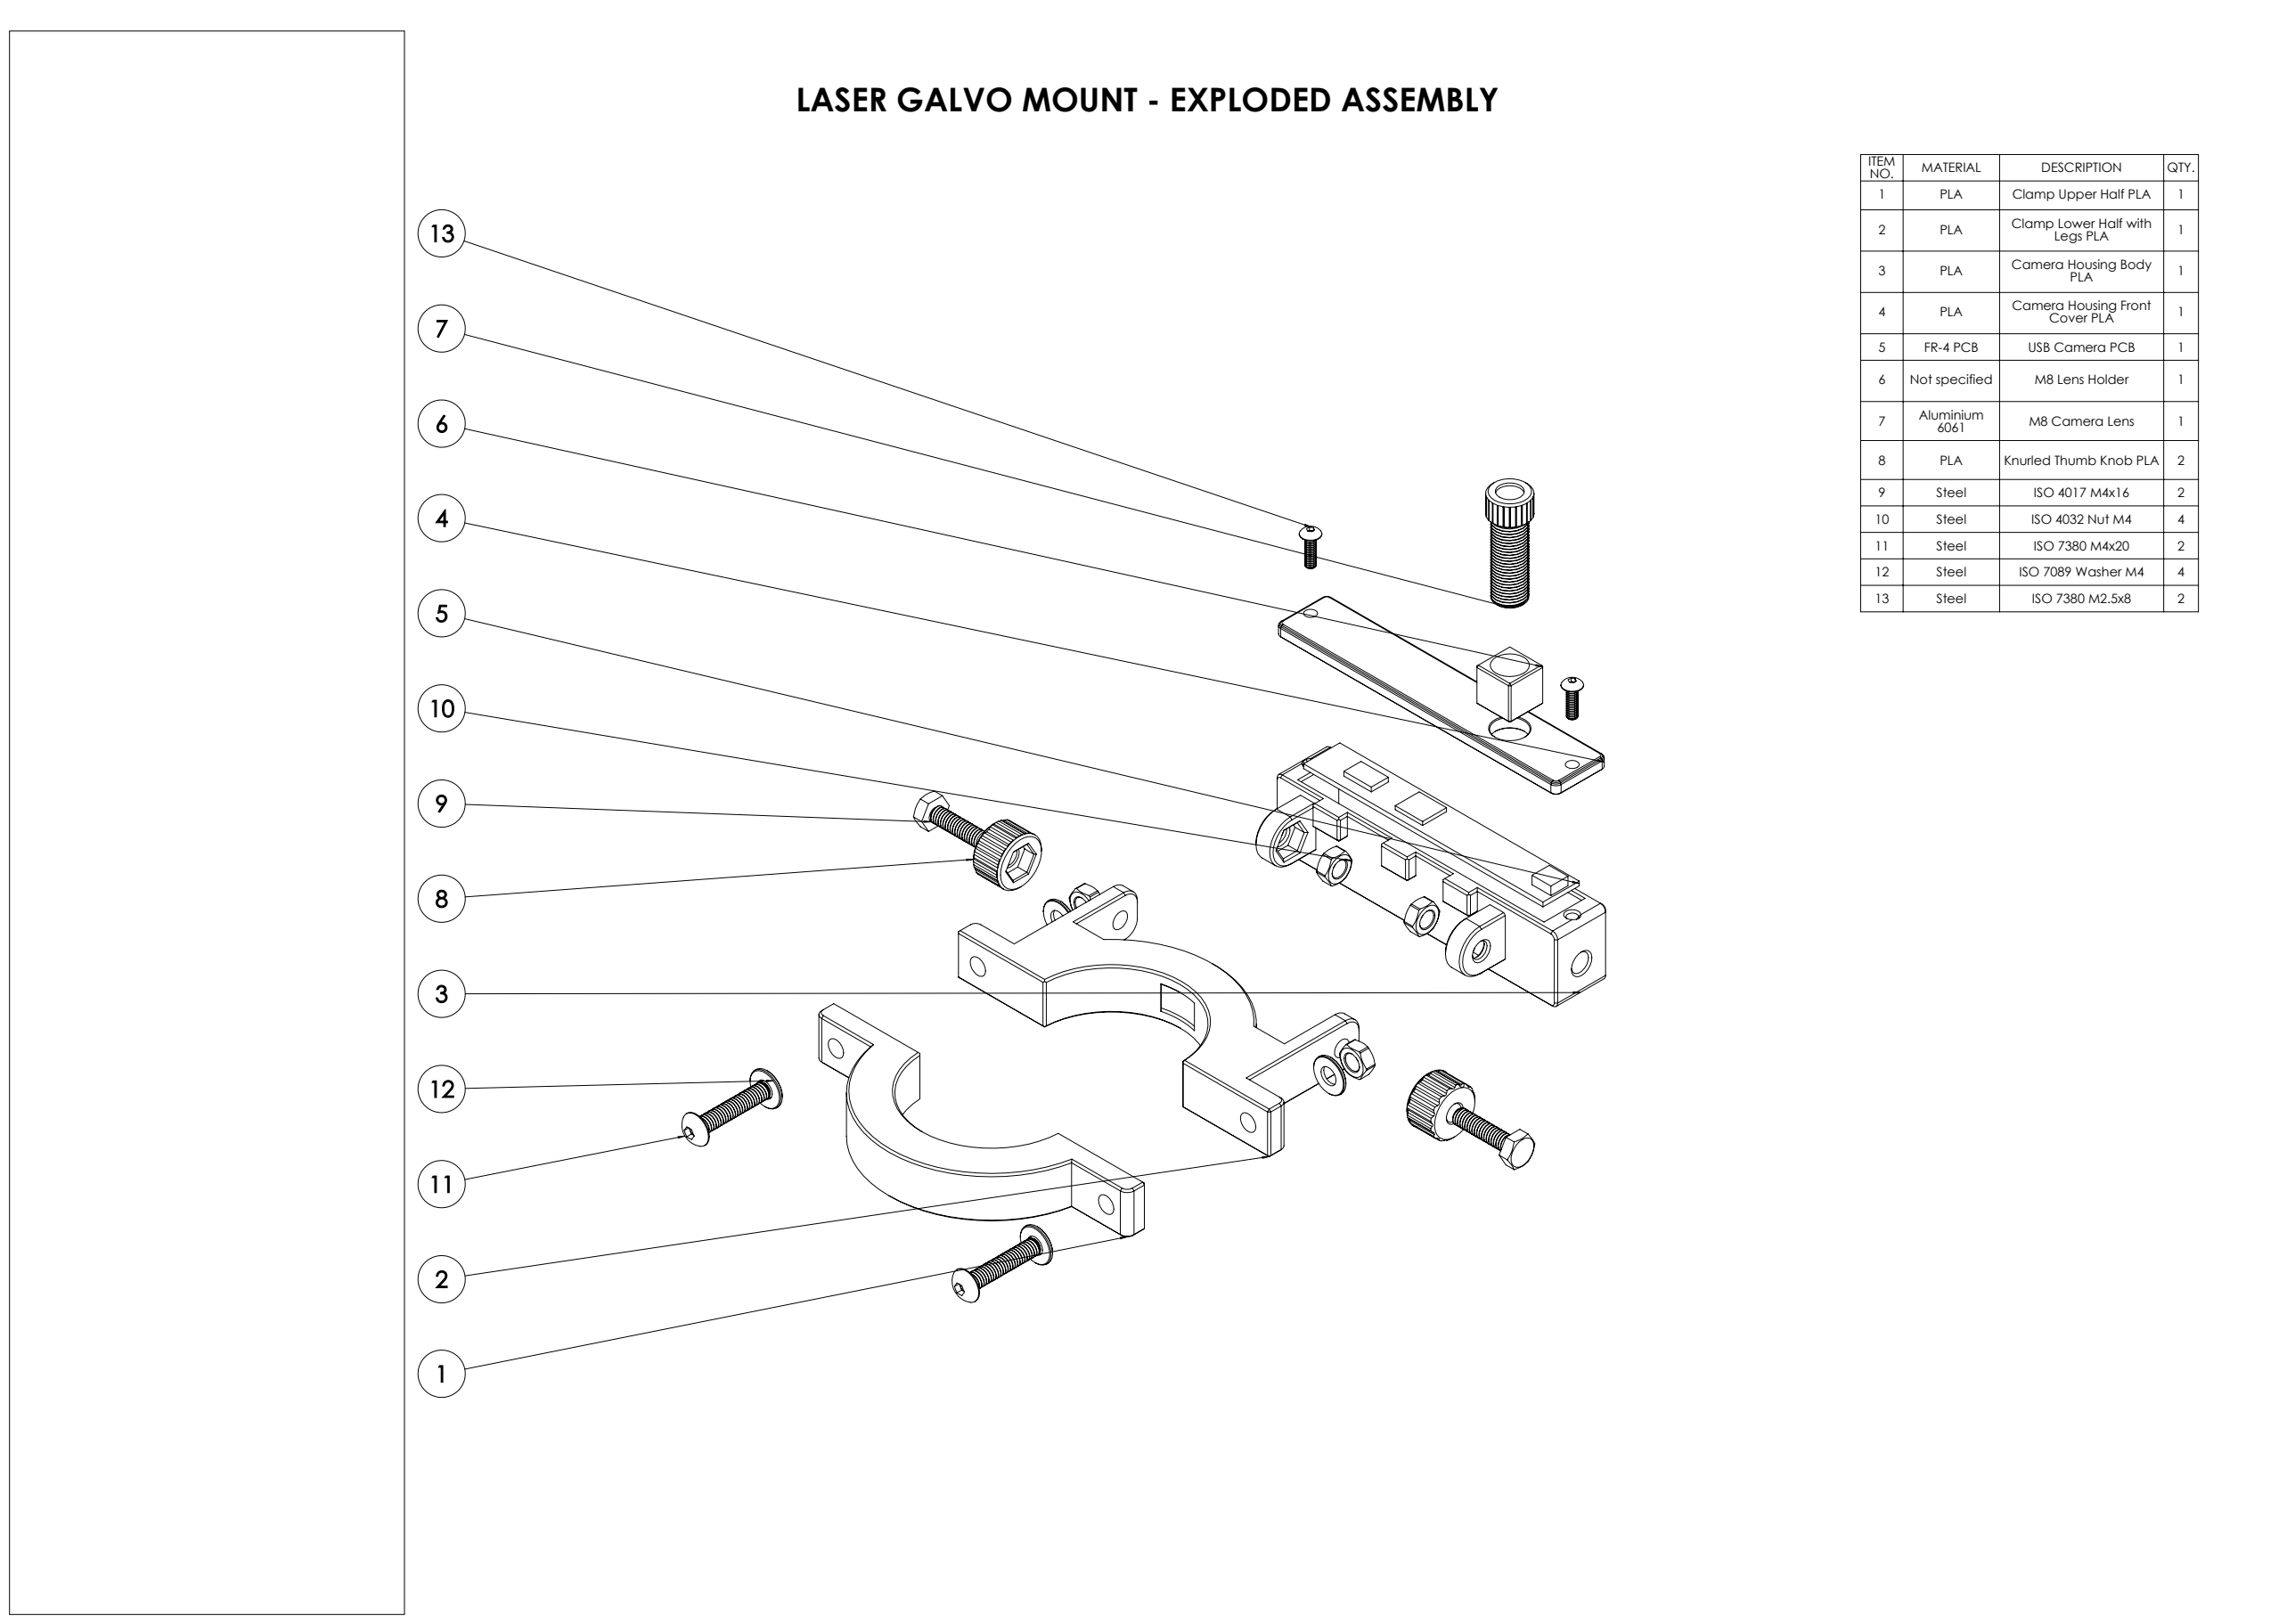
ISO-10303-21;
HEADER;
/* Generated by software containing ST-Developer
 * from STEP Tools, Inc. (www.steptools.com) 
 */

FILE_DESCRIPTION(
/* description */ (''),
/* implementation_level */ '2;1');

FILE_NAME(
/* name */ 'MAS-287',
/* time_stamp */ '2026-10-21T02:01:14-07:00',
/* author */ (''),
/* organization */ (''),
/* preprocessor_version */ 'ST-DEVELOPER v20.2',
/* originating_system */ 'Autodesk Translation Framework v15.15.0.0',
/* authorisation */ '');

FILE_SCHEMA (('AUTOMOTIVE_DESIGN { 1 0 10303 214 3 1 1 }'));
ENDSEC;

DATA;
#10=MECHANICAL_DESIGN_GEOMETRIC_PRESENTATION_REPRESENTATION('',(#614,#615,
#616,#617,#618,#619,#620,#621,#622,#623,#624,#625,#626),#37181);
#11=ITEM_DEFINED_TRANSFORMATION($,$,#14934,#16102);
#12=ITEM_DEFINED_TRANSFORMATION($,$,#14997,#16103);
#13=ITEM_DEFINED_TRANSFORMATION($,$,#15137,#16104);
#14=ITEM_DEFINED_TRANSFORMATION($,$,#15323,#16105);
#15=ITEM_DEFINED_TRANSFORMATION($,$,#15403,#16106);
#16=ITEM_DEFINED_TRANSFORMATION($,$,#15425,#16107);
#17=ITEM_DEFINED_TRANSFORMATION($,$,#15455,#16108);
#18=ITEM_DEFINED_TRANSFORMATION($,$,#15705,#16109);
#19=ITEM_DEFINED_TRANSFORMATION($,$,#15848,#16110);
#20=ITEM_DEFINED_TRANSFORMATION($,$,#16013,#16111);
#21=ITEM_DEFINED_TRANSFORMATION($,$,#15999,#16112);
#22=ITEM_DEFINED_TRANSFORMATION($,$,#15916,#16113);
#23=ITEM_DEFINED_TRANSFORMATION($,$,#15999,#16114);
#24=ITEM_DEFINED_TRANSFORMATION($,$,#16013,#16115);
#25=ITEM_DEFINED_TRANSFORMATION($,$,#15705,#16116);
#26=ITEM_DEFINED_TRANSFORMATION($,$,#15848,#16117);
#27=ITEM_DEFINED_TRANSFORMATION($,$,#16013,#16118);
#28=ITEM_DEFINED_TRANSFORMATION($,$,#15999,#16119);
#29=ITEM_DEFINED_TRANSFORMATION($,$,#15916,#16120);
#30=ITEM_DEFINED_TRANSFORMATION($,$,#15999,#16121);
#31=ITEM_DEFINED_TRANSFORMATION($,$,#16013,#16122);
#32=ITEM_DEFINED_TRANSFORMATION($,$,#16039,#16123);
#33=ITEM_DEFINED_TRANSFORMATION($,$,#16039,#16124);
#34=(
REPRESENTATION_RELATIONSHIP($,$,#37238,#37237)
REPRESENTATION_RELATIONSHIP_WITH_TRANSFORMATION(#11)
SHAPE_REPRESENTATION_RELATIONSHIP()
);
#35=(
REPRESENTATION_RELATIONSHIP($,$,#37239,#37237)
REPRESENTATION_RELATIONSHIP_WITH_TRANSFORMATION(#12)
SHAPE_REPRESENTATION_RELATIONSHIP()
);
#36=(
REPRESENTATION_RELATIONSHIP($,$,#37240,#37237)
REPRESENTATION_RELATIONSHIP_WITH_TRANSFORMATION(#13)
SHAPE_REPRESENTATION_RELATIONSHIP()
);
#37=(
REPRESENTATION_RELATIONSHIP($,$,#37241,#37237)
REPRESENTATION_RELATIONSHIP_WITH_TRANSFORMATION(#14)
SHAPE_REPRESENTATION_RELATIONSHIP()
);
#38=(
REPRESENTATION_RELATIONSHIP($,$,#37242,#37237)
REPRESENTATION_RELATIONSHIP_WITH_TRANSFORMATION(#15)
SHAPE_REPRESENTATION_RELATIONSHIP()
);
#39=(
REPRESENTATION_RELATIONSHIP($,$,#37243,#37237)
REPRESENTATION_RELATIONSHIP_WITH_TRANSFORMATION(#16)
SHAPE_REPRESENTATION_RELATIONSHIP()
);
#40=(
REPRESENTATION_RELATIONSHIP($,$,#37244,#37237)
REPRESENTATION_RELATIONSHIP_WITH_TRANSFORMATION(#17)
SHAPE_REPRESENTATION_RELATIONSHIP()
);
#41=(
REPRESENTATION_RELATIONSHIP($,$,#37245,#37237)
REPRESENTATION_RELATIONSHIP_WITH_TRANSFORMATION(#18)
SHAPE_REPRESENTATION_RELATIONSHIP()
);
#42=(
REPRESENTATION_RELATIONSHIP($,$,#37246,#37237)
REPRESENTATION_RELATIONSHIP_WITH_TRANSFORMATION(#19)
SHAPE_REPRESENTATION_RELATIONSHIP()
);
#43=(
REPRESENTATION_RELATIONSHIP($,$,#37249,#37237)
REPRESENTATION_RELATIONSHIP_WITH_TRANSFORMATION(#20)
SHAPE_REPRESENTATION_RELATIONSHIP()
);
#44=(
REPRESENTATION_RELATIONSHIP($,$,#37248,#37237)
REPRESENTATION_RELATIONSHIP_WITH_TRANSFORMATION(#21)
SHAPE_REPRESENTATION_RELATIONSHIP()
);
#45=(
REPRESENTATION_RELATIONSHIP($,$,#37247,#37237)
REPRESENTATION_RELATIONSHIP_WITH_TRANSFORMATION(#22)
SHAPE_REPRESENTATION_RELATIONSHIP()
);
#46=(
REPRESENTATION_RELATIONSHIP($,$,#37248,#37237)
REPRESENTATION_RELATIONSHIP_WITH_TRANSFORMATION(#23)
SHAPE_REPRESENTATION_RELATIONSHIP()
);
#47=(
REPRESENTATION_RELATIONSHIP($,$,#37249,#37237)
REPRESENTATION_RELATIONSHIP_WITH_TRANSFORMATION(#24)
SHAPE_REPRESENTATION_RELATIONSHIP()
);
#48=(
REPRESENTATION_RELATIONSHIP($,$,#37245,#37237)
REPRESENTATION_RELATIONSHIP_WITH_TRANSFORMATION(#25)
SHAPE_REPRESENTATION_RELATIONSHIP()
);
#49=(
REPRESENTATION_RELATIONSHIP($,$,#37246,#37237)
REPRESENTATION_RELATIONSHIP_WITH_TRANSFORMATION(#26)
SHAPE_REPRESENTATION_RELATIONSHIP()
);
#50=(
REPRESENTATION_RELATIONSHIP($,$,#37249,#37237)
REPRESENTATION_RELATIONSHIP_WITH_TRANSFORMATION(#27)
SHAPE_REPRESENTATION_RELATIONSHIP()
);
#51=(
REPRESENTATION_RELATIONSHIP($,$,#37248,#37237)
REPRESENTATION_RELATIONSHIP_WITH_TRANSFORMATION(#28)
SHAPE_REPRESENTATION_RELATIONSHIP()
);
#52=(
REPRESENTATION_RELATIONSHIP($,$,#37247,#37237)
REPRESENTATION_RELATIONSHIP_WITH_TRANSFORMATION(#29)
SHAPE_REPRESENTATION_RELATIONSHIP()
);
#53=(
REPRESENTATION_RELATIONSHIP($,$,#37248,#37237)
REPRESENTATION_RELATIONSHIP_WITH_TRANSFORMATION(#30)
SHAPE_REPRESENTATION_RELATIONSHIP()
);
#54=(
REPRESENTATION_RELATIONSHIP($,$,#37249,#37237)
REPRESENTATION_RELATIONSHIP_WITH_TRANSFORMATION(#31)
SHAPE_REPRESENTATION_RELATIONSHIP()
);
#55=(
REPRESENTATION_RELATIONSHIP($,$,#37250,#37237)
REPRESENTATION_RELATIONSHIP_WITH_TRANSFORMATION(#32)
SHAPE_REPRESENTATION_RELATIONSHIP()
);
#56=(
REPRESENTATION_RELATIONSHIP($,$,#37250,#37237)
REPRESENTATION_RELATIONSHIP_WITH_TRANSFORMATION(#33)
SHAPE_REPRESENTATION_RELATIONSHIP()
);
#57=CONTEXT_DEPENDENT_SHAPE_REPRESENTATION(#34,#37214);
#58=CONTEXT_DEPENDENT_SHAPE_REPRESENTATION(#35,#37215);
#59=CONTEXT_DEPENDENT_SHAPE_REPRESENTATION(#36,#37216);
#60=CONTEXT_DEPENDENT_SHAPE_REPRESENTATION(#37,#37217);
#61=CONTEXT_DEPENDENT_SHAPE_REPRESENTATION(#38,#37218);
#62=CONTEXT_DEPENDENT_SHAPE_REPRESENTATION(#39,#37219);
#63=CONTEXT_DEPENDENT_SHAPE_REPRESENTATION(#40,#37220);
#64=CONTEXT_DEPENDENT_SHAPE_REPRESENTATION(#41,#37221);
#65=CONTEXT_DEPENDENT_SHAPE_REPRESENTATION(#42,#37222);
#66=CONTEXT_DEPENDENT_SHAPE_REPRESENTATION(#43,#37223);
#67=CONTEXT_DEPENDENT_SHAPE_REPRESENTATION(#44,#37224);
#68=CONTEXT_DEPENDENT_SHAPE_REPRESENTATION(#45,#37225);
#69=CONTEXT_DEPENDENT_SHAPE_REPRESENTATION(#46,#37226);
#70=CONTEXT_DEPENDENT_SHAPE_REPRESENTATION(#47,#37227);
#71=CONTEXT_DEPENDENT_SHAPE_REPRESENTATION(#48,#37228);
#72=CONTEXT_DEPENDENT_SHAPE_REPRESENTATION(#49,#37229);
#73=CONTEXT_DEPENDENT_SHAPE_REPRESENTATION(#50,#37230);
#74=CONTEXT_DEPENDENT_SHAPE_REPRESENTATION(#51,#37231);
#75=CONTEXT_DEPENDENT_SHAPE_REPRESENTATION(#52,#37232);
#76=CONTEXT_DEPENDENT_SHAPE_REPRESENTATION(#53,#37233);
#77=CONTEXT_DEPENDENT_SHAPE_REPRESENTATION(#54,#37234);
#78=CONTEXT_DEPENDENT_SHAPE_REPRESENTATION(#55,#37235);
#79=CONTEXT_DEPENDENT_SHAPE_REPRESENTATION(#56,#37236);
#80=NEXT_ASSEMBLY_USAGE_OCCURRENCE('01_Clamp_Upper_Half_PLA:1',
'01_Clamp_Upper_Half_PLA:1','01_Clamp_Upper_Half_PLA:1',#37252,#37253,
'01_Clamp_Upper_Half_PLA:1');
#81=NEXT_ASSEMBLY_USAGE_OCCURRENCE(
'02_Clamp_Lower_Half_with_Legs_PLA:1',
'02_Clamp_Lower_Half_with_Legs_PLA:1',
'02_Clamp_Lower_Half_with_Legs_PLA:1',#37252,#37254,
'02_Clamp_Lower_Half_with_Legs_PLA:1');
#82=NEXT_ASSEMBLY_USAGE_OCCURRENCE('03_Camera_Housing_Body_PLA:1',
'03_Camera_Housing_Body_PLA:1','03_Camera_Housing_Body_PLA:1',#37252,#37255,
'03_Camera_Housing_Body_PLA:1');
#83=NEXT_ASSEMBLY_USAGE_OCCURRENCE(
'04_Camera_Housing_Front_Cover_PLA:1',
'04_Camera_Housing_Front_Cover_PLA:1',
'04_Camera_Housing_Front_Cover_PLA:1',#37252,#37256,
'04_Camera_Housing_Front_Cover_PLA:1');
#84=NEXT_ASSEMBLY_USAGE_OCCURRENCE('05_USB_Camera_PCB:1',
'05_USB_Camera_PCB:1','05_USB_Camera_PCB:1',#37252,#37257,
'05_USB_Camera_PCB:1');
#85=NEXT_ASSEMBLY_USAGE_OCCURRENCE('06_M8_Lens_Holder:1',
'06_M8_Lens_Holder:1','06_M8_Lens_Holder:1',#37252,#37258,
'06_M8_Lens_Holder:1');
#86=NEXT_ASSEMBLY_USAGE_OCCURRENCE('07_M8_Camera_Lens:2',
'07_M8_Camera_Lens:2','07_M8_Camera_Lens:2',#37252,#37259,
'07_M8_Camera_Lens:2');
#87=NEXT_ASSEMBLY_USAGE_OCCURRENCE('08_Knurled_Thumb_Knob_PLA:2',
'08_Knurled_Thumb_Knob_PLA:2','08_Knurled_Thumb_Knob_PLA:2',#37252,#37260,
'08_Knurled_Thumb_Knob_PLA:2');
#88=NEXT_ASSEMBLY_USAGE_OCCURRENCE('09_ISO_4017_M4x16:2',
'09_ISO_4017_M4x16:2','09_ISO_4017_M4x16:2',#37252,#37261,
'09_ISO_4017_M4x16:2');
#89=NEXT_ASSEMBLY_USAGE_OCCURRENCE('10_ISO_4032_Nut_M4:2',
'10_ISO_4032_Nut_M4:2','10_ISO_4032_Nut_M4:2',#37252,#37264,
'10_ISO_4032_Nut_M4:2');
#90=NEXT_ASSEMBLY_USAGE_OCCURRENCE('12_ISO_7089_Washer_M4:2',
'12_ISO_7089_Washer_M4:2','12_ISO_7089_Washer_M4:2',#37252,#37263,
'12_ISO_7089_Washer_M4:2');
#91=NEXT_ASSEMBLY_USAGE_OCCURRENCE('11_ISO_7380_M4x20:2',
'11_ISO_7380_M4x20:2','11_ISO_7380_M4x20:2',#37252,#37262,
'11_ISO_7380_M4x20:2');
#92=NEXT_ASSEMBLY_USAGE_OCCURRENCE('12_ISO_7089_Washer_M4:3',
'12_ISO_7089_Washer_M4:3','12_ISO_7089_Washer_M4:3',#37252,#37263,
'12_ISO_7089_Washer_M4:3');
#93=NEXT_ASSEMBLY_USAGE_OCCURRENCE('10_ISO_4032_Nut_M4:3',
'10_ISO_4032_Nut_M4:3','10_ISO_4032_Nut_M4:3',#37252,#37264,
'10_ISO_4032_Nut_M4:3');
#94=NEXT_ASSEMBLY_USAGE_OCCURRENCE('08_Knurled_Thumb_Knob_PLA:3',
'08_Knurled_Thumb_Knob_PLA:3','08_Knurled_Thumb_Knob_PLA:3',#37252,#37260,
'08_Knurled_Thumb_Knob_PLA:3');
#95=NEXT_ASSEMBLY_USAGE_OCCURRENCE('09_ISO_4017_M4x16:3',
'09_ISO_4017_M4x16:3','09_ISO_4017_M4x16:3',#37252,#37261,
'09_ISO_4017_M4x16:3');
#96=NEXT_ASSEMBLY_USAGE_OCCURRENCE('10_ISO_4032_Nut_M4:4',
'10_ISO_4032_Nut_M4:4','10_ISO_4032_Nut_M4:4',#37252,#37264,
'10_ISO_4032_Nut_M4:4');
#97=NEXT_ASSEMBLY_USAGE_OCCURRENCE('12_ISO_7089_Washer_M4:4',
'12_ISO_7089_Washer_M4:4','12_ISO_7089_Washer_M4:4',#37252,#37263,
'12_ISO_7089_Washer_M4:4');
#98=NEXT_ASSEMBLY_USAGE_OCCURRENCE('11_ISO_7380_M4x20:3',
'11_ISO_7380_M4x20:3','11_ISO_7380_M4x20:3',#37252,#37262,
'11_ISO_7380_M4x20:3');
#99=NEXT_ASSEMBLY_USAGE_OCCURRENCE('12_ISO_7089_Washer_M4:5',
'12_ISO_7089_Washer_M4:5','12_ISO_7089_Washer_M4:5',#37252,#37263,
'12_ISO_7089_Washer_M4:5');
#100=NEXT_ASSEMBLY_USAGE_OCCURRENCE('10_ISO_4032_Nut_M4:5',
'10_ISO_4032_Nut_M4:5','10_ISO_4032_Nut_M4:5',#37252,#37264,
'10_ISO_4032_Nut_M4:5');
#101=NEXT_ASSEMBLY_USAGE_OCCURRENCE('13_ISO_7380_M2.5x8:2',
'13_ISO_7380_M2.5x8:2','13_ISO_7380_M2.5x8:2',#37252,#37265,
'13_ISO_7380_M2.5x8:2');
#102=NEXT_ASSEMBLY_USAGE_OCCURRENCE('13_ISO_7380_M2.5x8:3',
'13_ISO_7380_M2.5x8:3','13_ISO_7380_M2.5x8:3',#37252,#37265,
'13_ISO_7380_M2.5x8:3');
#103=(
BOUNDED_SURFACE()
B_SPLINE_SURFACE(2,2,((#34249,#34250,#34251,#34252,#34253,#34254,#34255,
#34256,#34257),(#34258,#34259,#34260,#34261,#34262,#34263,#34264,#34265,
#34266),(#34267,#34268,#34269,#34270,#34271,#34272,#34273,#34274,#34275)),
 .UNSPECIFIED.,.F.,.T.,.F.)
B_SPLINE_SURFACE_WITH_KNOTS((3,3),(3,2,2,2,3),(0.516279708895519,1.35421937474488),
(-3.14159265358979,-1.5707963267949,0.,1.5707963267949,3.14159265358979),
 .UNSPECIFIED.)
GEOMETRIC_REPRESENTATION_ITEM()
RATIONAL_B_SPLINE_SURFACE(((1.,0.707106781186548,1.,0.707106781186548,1.,
0.707106781186548,1.,0.707106781186548,1.),(0.91350851712624,0.645948067131631,
0.91350851712624,0.645948067131631,0.91350851712624,0.645948067131631,0.91350851712624,
0.645948067131631,0.91350851712624),(1.,0.707106781186548,1.,0.707106781186548,
1.,0.707106781186548,1.,0.707106781186548,1.)))
REPRESENTATION_ITEM('')
SURFACE()
);
#104=(
BOUNDED_SURFACE()
B_SPLINE_SURFACE(2,2,((#37099,#37100,#37101,#37102,#37103,#37104,#37105,
#37106,#37107),(#37108,#37109,#37110,#37111,#37112,#37113,#37114,#37115,
#37116),(#37117,#37118,#37119,#37120,#37121,#37122,#37123,#37124,#37125)),
 .UNSPECIFIED.,.F.,.T.,.F.)
B_SPLINE_SURFACE_WITH_KNOTS((3,3),(3,2,2,2,3),(0.513408172091738,1.39168804086818),
(-3.14159265358979,-1.5707963267949,0.,1.5707963267949,3.14159265358979),
 .UNSPECIFIED.)
GEOMETRIC_REPRESENTATION_ITEM()
RATIONAL_B_SPLINE_SURFACE(((1.,0.707106781186548,1.,0.707106781186548,1.,
0.707106781186548,1.,0.707106781186548,1.),(0.905117664433204,0.640014838292448,
0.905117664433204,0.640014838292448,0.905117664433204,0.640014838292448,
0.905117664433204,0.640014838292448,0.905117664433204),(1.,0.707106781186548,
1.,0.707106781186548,1.,0.707106781186548,1.,0.707106781186548,1.)))
REPRESENTATION_ITEM('')
SURFACE()
);
#105=B_SPLINE_SURFACE_WITH_KNOTS('',3,3,((#21181,#21182,#21183,#21184,#21185,
#21186),(#21187,#21188,#21189,#21190,#21191,#21192),(#21193,#21194,#21195,
#21196,#21197,#21198),(#21199,#21200,#21201,#21202,#21203,#21204)),
 .UNSPECIFIED.,.F.,.F.,.F.,(4,4),(4,2,4),(0.,1.),(0.268796457448958,0.30404357328347,
0.339290689117984),.UNSPECIFIED.);
#106=B_SPLINE_SURFACE_WITH_KNOTS('',3,3,((#21223,#21224,#21225,#21226),
(#21227,#21228,#21229,#21230),(#21231,#21232,#21233,#21234),(#21235,#21236,
#21237,#21238)),.UNSPECIFIED.,.F.,.F.,.F.,(4,4),(4,4),(0.,1.),(0.278246822734795,
0.803148805386868),.UNSPECIFIED.);
#107=B_SPLINE_SURFACE_WITH_KNOTS('',3,3,((#21243,#21244,#21245,#21246),
(#21247,#21248,#21249,#21250),(#21251,#21252,#21253,#21254),(#21255,#21256,
#21257,#21258)),.UNSPECIFIED.,.F.,.F.,.F.,(4,4),(4,4),(0.,1.),(-0.803148805386867,
-0.278246822734795),.UNSPECIFIED.);
#108=B_SPLINE_SURFACE_WITH_KNOTS('',3,3,((#21267,#21268,#21269,#21270,#21271,
#21272),(#21273,#21274,#21275,#21276,#21277,#21278),(#21279,#21280,#21281,
#21282,#21283,#21284),(#21285,#21286,#21287,#21288,#21289,#21290)),
 .UNSPECIFIED.,.F.,.F.,.F.,(4,4),(4,2,4),(0.,1.),(0.268796457448958,0.304043573283469,
0.33929068911798),.UNSPECIFIED.);
#109=B_SPLINE_SURFACE_WITH_KNOTS('',3,3,((#21310,#21311,#21312,#21313),
(#21314,#21315,#21316,#21317),(#21318,#21319,#21320,#21321),(#21322,#21323,
#21324,#21325)),.UNSPECIFIED.,.F.,.F.,.F.,(4,4),(4,4),(0.,1.),(-2.86334583085503,
-2.33844384820293),.UNSPECIFIED.);
#110=B_SPLINE_SURFACE_WITH_KNOTS('',3,3,((#21330,#21331,#21332,#21333),
(#21334,#21335,#21336,#21337),(#21338,#21339,#21340,#21341),(#21342,#21343,
#21344,#21345)),.UNSPECIFIED.,.F.,.F.,.F.,(4,4),(4,4),(0.,1.),(-3.94474145897665,
-3.41983947632457),.UNSPECIFIED.);
#111=B_SPLINE_SURFACE_WITH_KNOTS('',3,3,((#24257,#24258,#24259,#24260,#24261,
#24262,#24263,#24264,#24265,#24266,#24267,#24268,#24269,#24270,#24271,#24272,
#24273,#24274,#24275,#24276,#24277,#24278,#24279,#24280,#24281,#24282,#24283,
#24284,#24285,#24286,#24287,#24288,#24289,#24290,#24291,#24292,#24293,#24294,
#24295,#24296,#24297,#24298,#24299,#24300,#24301,#24302,#24303,#24304,#24305,
#24306,#24307,#24308,#24309,#24310,#24311,#24312,#24313,#24314,#24315,#24316,
#24317,#24318,#24319,#24320,#24321,#24322,#24323,#24324,#24325,#24326,#24327,
#24328,#24329,#24330,#24331,#24332,#24333,#24334,#24335,#24336,#24337,#24338,
#24339,#24340,#24341,#24342,#24343,#24344,#24345,#24346,#24347,#24348,#24349,
#24350,#24351,#24352,#24353,#24354,#24355,#24356,#24357,#24358,#24359,#24360,
#24361,#24362,#24363,#24364,#24365,#24366,#24367,#24368,#24369,#24370,#24371,
#24372,#24373,#24374,#24375,#24376,#24377,#24378,#24379,#24380,#24381,#24382,
#24383,#24384,#24385,#24386,#24387,#24388,#24389,#24390,#24391,#24392,#24393,
#24394,#24395,#24396,#24397,#24398,#24399,#24400,#24401,#24402,#24403,#24404,
#24405,#24406,#24407,#24408,#24409,#24410,#24411,#24412,#24413,#24414,#24415,
#24416,#24417,#24418,#24419,#24420,#24421,#24422,#24423,#24424,#24425,#24426,
#24427,#24428,#24429,#24430,#24431,#24432,#24433,#24434,#24435),(#24436,
#24437,#24438,#24439,#24440,#24441,#24442,#24443,#24444,#24445,#24446,#24447,
#24448,#24449,#24450,#24451,#24452,#24453,#24454,#24455,#24456,#24457,#24458,
#24459,#24460,#24461,#24462,#24463,#24464,#24465,#24466,#24467,#24468,#24469,
#24470,#24471,#24472,#24473,#24474,#24475,#24476,#24477,#24478,#24479,#24480,
#24481,#24482,#24483,#24484,#24485,#24486,#24487,#24488,#24489,#24490,#24491,
#24492,#24493,#24494,#24495,#24496,#24497,#24498,#24499,#24500,#24501,#24502,
#24503,#24504,#24505,#24506,#24507,#24508,#24509,#24510,#24511,#24512,#24513,
#24514,#24515,#24516,#24517,#24518,#24519,#24520,#24521,#24522,#24523,#24524,
#24525,#24526,#24527,#24528,#24529,#24530,#24531,#24532,#24533,#24534,#24535,
#24536,#24537,#24538,#24539,#24540,#24541,#24542,#24543,#24544,#24545,#24546,
#24547,#24548,#24549,#24550,#24551,#24552,#24553,#24554,#24555,#24556,#24557,
#24558,#24559,#24560,#24561,#24562,#24563,#24564,#24565,#24566,#24567,#24568,
#24569,#24570,#24571,#24572,#24573,#24574,#24575,#24576,#24577,#24578,#24579,
#24580,#24581,#24582,#24583,#24584,#24585,#24586,#24587,#24588,#24589,#24590,
#24591,#24592,#24593,#24594,#24595,#24596,#24597,#24598,#24599,#24600,#24601,
#24602,#24603,#24604,#24605,#24606,#24607,#24608,#24609,#24610,#24611,#24612,
#24613,#24614),(#24615,#24616,#24617,#24618,#24619,#24620,#24621,#24622,
#24623,#24624,#24625,#24626,#24627,#24628,#24629,#24630,#24631,#24632,#24633,
#24634,#24635,#24636,#24637,#24638,#24639,#24640,#24641,#24642,#24643,#24644,
#24645,#24646,#24647,#24648,#24649,#24650,#24651,#24652,#24653,#24654,#24655,
#24656,#24657,#24658,#24659,#24660,#24661,#24662,#24663,#24664,#24665,#24666,
#24667,#24668,#24669,#24670,#24671,#24672,#24673,#24674,#24675,#24676,#24677,
#24678,#24679,#24680,#24681,#24682,#24683,#24684,#24685,#24686,#24687,#24688,
#24689,#24690,#24691,#24692,#24693,#24694,#24695,#24696,#24697,#24698,#24699,
#24700,#24701,#24702,#24703,#24704,#24705,#24706,#24707,#24708,#24709,#24710,
#24711,#24712,#24713,#24714,#24715,#24716,#24717,#24718,#24719,#24720,#24721,
#24722,#24723,#24724,#24725,#24726,#24727,#24728,#24729,#24730,#24731,#24732,
#24733,#24734,#24735,#24736,#24737,#24738,#24739,#24740,#24741,#24742,#24743,
#24744,#24745,#24746,#24747,#24748,#24749,#24750,#24751,#24752,#24753,#24754,
#24755,#24756,#24757,#24758,#24759,#24760,#24761,#24762,#24763,#24764,#24765,
#24766,#24767,#24768,#24769,#24770,#24771,#24772,#24773,#24774,#24775,#24776,
#24777,#24778,#24779,#24780,#24781,#24782,#24783,#24784,#24785,#24786,#24787,
#24788,#24789,#24790,#24791,#24792,#24793),(#24794,#24795,#24796,#24797,
#24798,#24799,#24800,#24801,#24802,#24803,#24804,#24805,#24806,#24807,#24808,
#24809,#24810,#24811,#24812,#24813,#24814,#24815,#24816,#24817,#24818,#24819,
#24820,#24821,#24822,#24823,#24824,#24825,#24826,#24827,#24828,#24829,#24830,
#24831,#24832,#24833,#24834,#24835,#24836,#24837,#24838,#24839,#24840,#24841,
#24842,#24843,#24844,#24845,#24846,#24847,#24848,#24849,#24850,#24851,#24852,
#24853,#24854,#24855,#24856,#24857,#24858,#24859,#24860,#24861,#24862,#24863,
#24864,#24865,#24866,#24867,#24868,#24869,#24870,#24871,#24872,#24873,#24874,
#24875,#24876,#24877,#24878,#24879,#24880,#24881,#24882,#24883,#24884,#24885,
#24886,#24887,#24888,#24889,#24890,#24891,#24892,#24893,#24894,#24895,#24896,
#24897,#24898,#24899,#24900,#24901,#24902,#24903,#24904,#24905,#24906,#24907,
#24908,#24909,#24910,#24911,#24912,#24913,#24914,#24915,#24916,#24917,#24918,
#24919,#24920,#24921,#24922,#24923,#24924,#24925,#24926,#24927,#24928,#24929,
#24930,#24931,#24932,#24933,#24934,#24935,#24936,#24937,#24938,#24939,#24940,
#24941,#24942,#24943,#24944,#24945,#24946,#24947,#24948,#24949,#24950,#24951,
#24952,#24953,#24954,#24955,#24956,#24957,#24958,#24959,#24960,#24961,#24962,
#24963,#24964,#24965,#24966,#24967,#24968,#24969,#24970,#24971,#24972)),
 .UNSPECIFIED.,.F.,.F.,.F.,(4,4),(4,1,1,1,1,1,1,1,1,1,1,1,1,1,1,1,1,1,1,
1,1,1,1,1,1,1,1,1,1,1,1,1,1,1,1,1,1,1,1,1,1,1,1,1,1,1,1,1,1,1,1,1,1,1,1,
1,1,1,1,1,1,1,1,1,1,1,1,1,1,1,1,1,1,1,1,1,1,1,1,1,1,1,1,1,1,1,1,1,1,1,1,
1,1,1,1,1,1,1,1,1,1,1,1,1,1,1,1,1,1,1,1,1,1,1,1,1,1,1,1,1,1,1,1,1,1,1,1,
1,1,1,1,1,1,1,1,1,1,1,1,1,1,1,1,1,1,1,1,1,1,1,1,1,1,1,1,1,1,1,1,1,1,1,1,
1,1,1,1,1,1,1,1,1,1,1,1,1,4),(0.,0.0496809906637673),(8.29514371672438,
9.2897150667619,10.2842864167994,11.2788577668369,12.2734291168745,13.268000466912,
14.2625718169495,15.257143166987,16.2517145170246,17.2462858670621,18.2408572170996,
19.2354285671371,20.2299999171747,21.2245712672122,22.2191426172497,23.2137139672872,
24.2082853173248,25.2028566673623,26.1974280173998,27.1919993674374,28.1865707174749,
29.1811420675124,30.1757134175499,31.1702847675875,32.164856117625,33.1594274676625,
34.1539988177,35.1485701677375,36.1431415177751,37.1377128678126,38.1322842178501,
39.1268555678876,40.1214269179252,41.1159982679627,42.1105696180002,43.1051409680378,
44.0997123180753,45.0942836681128,46.0888550181503,47.0834263681879,48.0779977182254,
49.0725690682629,50.0671404183004,51.061711768338,52.0562831183755,53.050854468413,
54.0454258184505,55.039997168488,56.0345685185256,57.0291398685631,58.0237112186006,
59.0182825686381,60.0128539186757,61.0074252687132,62.0019966187507,62.9965679687882,
63.9911393188258,64.9857106688633,65.9802820189008,66.9748533689383,67.9694247189759,
68.9639960690134,69.9585674190509,70.9531387690884,71.947710119126,72.9422814691635,
73.936852819201,74.9314241692385,75.9259955192761,76.9205668693136,77.9151382193511,
78.9097095693886,79.9042809194262,80.8988522694637,81.8934236195012,82.8879949695387,
83.8825663195763,84.8771376696138,85.8717090196513,86.8662803696888,87.8608517197264,
88.8554230697639,89.8499944198014,90.8445657698389,91.8391371198765,92.833708469914,
93.8282798199515,94.822851169989,95.8174225200266,96.8119938700641,97.8065652201016,
98.8011365701391,99.7957079201767,100.790279270214,101.784850620252,102.779421970289,
103.773993320327,104.768564670364,105.763136020402,106.757707370439,107.752278720477,
108.746850070514,109.741421420552,110.735992770589,111.730564120627,112.725135470664,
113.719706820702,114.71427817074,115.708849520777,116.703420870815,117.697992220852,
118.69256357089,119.687134920927,120.681706270965,121.676277621002,122.67084897104,
123.665420321077,124.659991671115,125.654563021152,126.64913437119,127.643705721227,
128.638277071265,129.632848421302,130.62741977134,131.621991121377,132.616562471415,
133.611133821453,134.60570517149,135.600276521528,136.594847871565,137.589419221603,
138.58399057164,139.578561921678,140.573133271715,141.567704621753,142.56227597179,
143.556847321828,144.551418671865,145.545990021903,146.54056137194,147.535132721978,
148.529704072015,149.524275422053,150.51884677209,151.513418122128,152.507989472165,
153.502560822203,154.497132172241,155.491703522278,156.486274872316,157.480846222353,
158.475417572391,159.469988922428,160.464560272466,161.459131622503,162.453702972541,
163.448274322578,164.442845672616,165.437417022653,166.431988372691,167.426559722728,
168.421131072766,169.415702422803,170.410273772841,171.404845122878,172.399416472916,
173.393987822954,174.388559172991,175.383130523029,176.377701873066,177.372273223104,
178.366844573141,179.361415923179,180.355987273216,181.350558623254,182.345129973291,
183.339701323329),.UNSPECIFIED.);
#112=B_SPLINE_SURFACE_WITH_KNOTS('',3,3,((#25202,#25203,#25204,#25205,#25206,
#25207,#25208,#25209,#25210,#25211,#25212,#25213,#25214,#25215,#25216,#25217,
#25218,#25219,#25220,#25221,#25222,#25223,#25224,#25225,#25226,#25227,#25228,
#25229,#25230,#25231,#25232,#25233,#25234,#25235,#25236,#25237,#25238,#25239,
#25240,#25241,#25242,#25243,#25244,#25245,#25246,#25247,#25248,#25249,#25250,
#25251,#25252,#25253,#25254,#25255,#25256,#25257,#25258,#25259,#25260,#25261,
#25262,#25263,#25264,#25265,#25266,#25267,#25268,#25269,#25270,#25271,#25272,
#25273,#25274,#25275,#25276,#25277,#25278,#25279,#25280,#25281,#25282,#25283,
#25284,#25285,#25286,#25287,#25288,#25289,#25290,#25291,#25292,#25293,#25294,
#25295,#25296,#25297,#25298,#25299,#25300,#25301,#25302,#25303,#25304,#25305,
#25306,#25307,#25308,#25309,#25310,#25311,#25312,#25313,#25314,#25315,#25316,
#25317,#25318,#25319,#25320,#25321,#25322,#25323,#25324,#25325,#25326,#25327,
#25328,#25329,#25330,#25331,#25332,#25333,#25334,#25335,#25336,#25337,#25338,
#25339,#25340,#25341,#25342,#25343,#25344,#25345,#25346,#25347,#25348,#25349,
#25350,#25351,#25352,#25353,#25354,#25355,#25356,#25357,#25358,#25359,#25360,
#25361,#25362,#25363,#25364,#25365,#25366,#25367,#25368,#25369,#25370,#25371,
#25372,#25373,#25374,#25375,#25376,#25377,#25378,#25379,#25380),(#25381,
#25382,#25383,#25384,#25385,#25386,#25387,#25388,#25389,#25390,#25391,#25392,
#25393,#25394,#25395,#25396,#25397,#25398,#25399,#25400,#25401,#25402,#25403,
#25404,#25405,#25406,#25407,#25408,#25409,#25410,#25411,#25412,#25413,#25414,
#25415,#25416,#25417,#25418,#25419,#25420,#25421,#25422,#25423,#25424,#25425,
#25426,#25427,#25428,#25429,#25430,#25431,#25432,#25433,#25434,#25435,#25436,
#25437,#25438,#25439,#25440,#25441,#25442,#25443,#25444,#25445,#25446,#25447,
#25448,#25449,#25450,#25451,#25452,#25453,#25454,#25455,#25456,#25457,#25458,
#25459,#25460,#25461,#25462,#25463,#25464,#25465,#25466,#25467,#25468,#25469,
#25470,#25471,#25472,#25473,#25474,#25475,#25476,#25477,#25478,#25479,#25480,
#25481,#25482,#25483,#25484,#25485,#25486,#25487,#25488,#25489,#25490,#25491,
#25492,#25493,#25494,#25495,#25496,#25497,#25498,#25499,#25500,#25501,#25502,
#25503,#25504,#25505,#25506,#25507,#25508,#25509,#25510,#25511,#25512,#25513,
#25514,#25515,#25516,#25517,#25518,#25519,#25520,#25521,#25522,#25523,#25524,
#25525,#25526,#25527,#25528,#25529,#25530,#25531,#25532,#25533,#25534,#25535,
#25536,#25537,#25538,#25539,#25540,#25541,#25542,#25543,#25544,#25545,#25546,
#25547,#25548,#25549,#25550,#25551,#25552,#25553,#25554,#25555,#25556,#25557,
#25558,#25559),(#25560,#25561,#25562,#25563,#25564,#25565,#25566,#25567,
#25568,#25569,#25570,#25571,#25572,#25573,#25574,#25575,#25576,#25577,#25578,
#25579,#25580,#25581,#25582,#25583,#25584,#25585,#25586,#25587,#25588,#25589,
#25590,#25591,#25592,#25593,#25594,#25595,#25596,#25597,#25598,#25599,#25600,
#25601,#25602,#25603,#25604,#25605,#25606,#25607,#25608,#25609,#25610,#25611,
#25612,#25613,#25614,#25615,#25616,#25617,#25618,#25619,#25620,#25621,#25622,
#25623,#25624,#25625,#25626,#25627,#25628,#25629,#25630,#25631,#25632,#25633,
#25634,#25635,#25636,#25637,#25638,#25639,#25640,#25641,#25642,#25643,#25644,
#25645,#25646,#25647,#25648,#25649,#25650,#25651,#25652,#25653,#25654,#25655,
#25656,#25657,#25658,#25659,#25660,#25661,#25662,#25663,#25664,#25665,#25666,
#25667,#25668,#25669,#25670,#25671,#25672,#25673,#25674,#25675,#25676,#25677,
#25678,#25679,#25680,#25681,#25682,#25683,#25684,#25685,#25686,#25687,#25688,
#25689,#25690,#25691,#25692,#25693,#25694,#25695,#25696,#25697,#25698,#25699,
#25700,#25701,#25702,#25703,#25704,#25705,#25706,#25707,#25708,#25709,#25710,
#25711,#25712,#25713,#25714,#25715,#25716,#25717,#25718,#25719,#25720,#25721,
#25722,#25723,#25724,#25725,#25726,#25727,#25728,#25729,#25730,#25731,#25732,
#25733,#25734,#25735,#25736,#25737,#25738),(#25739,#25740,#25741,#25742,
#25743,#25744,#25745,#25746,#25747,#25748,#25749,#25750,#25751,#25752,#25753,
#25754,#25755,#25756,#25757,#25758,#25759,#25760,#25761,#25762,#25763,#25764,
#25765,#25766,#25767,#25768,#25769,#25770,#25771,#25772,#25773,#25774,#25775,
#25776,#25777,#25778,#25779,#25780,#25781,#25782,#25783,#25784,#25785,#25786,
#25787,#25788,#25789,#25790,#25791,#25792,#25793,#25794,#25795,#25796,#25797,
#25798,#25799,#25800,#25801,#25802,#25803,#25804,#25805,#25806,#25807,#25808,
#25809,#25810,#25811,#25812,#25813,#25814,#25815,#25816,#25817,#25818,#25819,
#25820,#25821,#25822,#25823,#25824,#25825,#25826,#25827,#25828,#25829,#25830,
#25831,#25832,#25833,#25834,#25835,#25836,#25837,#25838,#25839,#25840,#25841,
#25842,#25843,#25844,#25845,#25846,#25847,#25848,#25849,#25850,#25851,#25852,
#25853,#25854,#25855,#25856,#25857,#25858,#25859,#25860,#25861,#25862,#25863,
#25864,#25865,#25866,#25867,#25868,#25869,#25870,#25871,#25872,#25873,#25874,
#25875,#25876,#25877,#25878,#25879,#25880,#25881,#25882,#25883,#25884,#25885,
#25886,#25887,#25888,#25889,#25890,#25891,#25892,#25893,#25894,#25895,#25896,
#25897,#25898,#25899,#25900,#25901,#25902,#25903,#25904,#25905,#25906,#25907,
#25908,#25909,#25910,#25911,#25912,#25913,#25914,#25915,#25916,#25917)),
 .UNSPECIFIED.,.F.,.F.,.F.,(4,4),(4,1,1,1,1,1,1,1,1,1,1,1,1,1,1,1,1,1,1,
1,1,1,1,1,1,1,1,1,1,1,1,1,1,1,1,1,1,1,1,1,1,1,1,1,1,1,1,1,1,1,1,1,1,1,1,
1,1,1,1,1,1,1,1,1,1,1,1,1,1,1,1,1,1,1,1,1,1,1,1,1,1,1,1,1,1,1,1,1,1,1,1,
1,1,1,1,1,1,1,1,1,1,1,1,1,1,1,1,1,1,1,1,1,1,1,1,1,1,1,1,1,1,1,1,1,1,1,1,
1,1,1,1,1,1,1,1,1,1,1,1,1,1,1,1,1,1,1,1,1,1,1,1,1,1,1,1,1,1,1,1,1,1,1,1,
1,1,1,1,1,1,1,1,1,1,1,1,1,4),(0.,0.0496809906637673),(11.6149723878396,
12.6095437378771,13.6041150879146,14.5986864379522,15.5932577879897,16.5878291380272,
17.5824004880647,18.5769718381023,19.5715431881398,20.5661145381773,21.5606858882148,
22.5552572382524,23.5498285882899,24.5443999383274,25.5389712883649,26.5335426384025,
27.52811398844,28.5226853384775,29.517256688515,30.5118280385526,31.5063993885901,
32.5009707386276,33.4955420886651,34.4901134387027,35.4846847887402,36.4792561387777,
37.4738274888152,38.4683988388528,39.4629701888903,40.4575415389278,41.4521128889653,
42.4466842390029,43.4412555890404,44.4358269390779,45.4303982891154,46.424969639153,
47.4195409891905,48.414112339228,49.4086836892655,50.4032550393031,51.3978263893406,
52.3923977393781,53.3869690894156,54.3815404394532,55.3761117894907,56.3706831395282,
57.3652544895657,58.3598258396033,59.3543971896408,60.3489685396783,61.3435398897158,
62.3381112397534,63.3326825897909,64.3272539398284,65.3218252898659,66.3163966399035,
67.310967989941,68.3055393399785,69.300110690016,70.2946820400536,71.2892533900911,
72.2838247401286,73.2783960901661,74.2729674402037,75.2675387902412,76.2621101402787,
77.2566814903162,78.2512528403538,79.2458241903913,80.2403955404288,81.2349668904663,
82.2295382405039,83.2241095905414,84.2186809405789,85.2132522906164,86.207823640654,
87.2023949906915,88.196966340729,89.1915376907665,90.1861090408041,91.1806803908416,
92.1752517408791,93.1698230909166,94.1643944409542,95.1589657909917,96.1535371410292,
97.1481084910667,98.1426798411043,99.1372511911418,100.131822541179,101.126393891217,
102.120965241254,103.115536591292,104.110107941329,105.104679291367,106.099250641404,
107.093821991442,108.08839334148,109.082964691517,110.077536041555,111.072107391592,
112.06667874163,113.061250091667,114.055821441705,115.050392791742,116.04496414178,
117.039535491817,118.034106841855,119.028678191892,120.02324954193,121.017820891967,
122.012392242005,123.006963592042,124.00153494208,124.996106292117,125.990677642155,
126.985248992192,127.97982034223,128.974391692268,129.968963042305,130.963534392343,
131.95810574238,132.952677092418,133.947248442455,134.941819792493,135.93639114253,
136.930962492568,137.925533842605,138.920105192643,139.91467654268,140.909247892718,
141.903819242755,142.898390592793,143.89296194283,144.887533292868,145.882104642905,
146.876675992943,147.87124734298,148.865818693018,149.860390043056,150.854961393093,
151.849532743131,152.844104093168,153.838675443206,154.833246793243,155.827818143281,
156.822389493318,157.816960843356,158.811532193393,159.806103543431,160.800674893468,
161.795246243506,162.789817593543,163.784388943581,164.778960293618,165.773531643656,
166.768102993693,167.762674343731,168.757245693769,169.751817043806,170.746388393844,
171.740959743881,172.735531093919,173.730102443956,174.724673793994,175.719245144031,
176.713816494069,177.708387844106,178.702959194144,179.697530544181,180.692101894219,
181.686673244256,182.681244594294,183.675815944331,184.670387294369,185.664958644406,
186.659529994444),.UNSPECIFIED.);
#113=B_SPLINE_SURFACE_WITH_KNOTS('',3,3,((#26771,#26772,#26773,#26774,#26775,
#26776,#26777,#26778,#26779),(#26780,#26781,#26782,#26783,#26784,#26785,
#26786,#26787,#26788),(#26789,#26790,#26791,#26792,#26793,#26794,#26795,
#26796,#26797),(#26798,#26799,#26800,#26801,#26802,#26803,#26804,#26805,
#26806)),.UNSPECIFIED.,.F.,.F.,.F.,(4,4),(4,1,1,1,1,1,4),(0.,1.),(0.0342009647377285,
0.0587640238978664,0.0833270830580044,0.107890142218142,0.13245320137828,
0.181579319698556,0.206142378858694),.UNSPECIFIED.);
#114=B_SPLINE_SURFACE_WITH_KNOTS('',3,3,((#28629,#28630,#28631,#28632,#28633,
#28634,#28635,#28636,#28637,#28638,#28639,#28640,#28641,#28642,#28643,#28644,
#28645,#28646,#28647,#28648,#28649,#28650,#28651,#28652,#28653,#28654,#28655,
#28656,#28657,#28658,#28659,#28660,#28661,#28662,#28663,#28664,#28665,#28666,
#28667,#28668,#28669,#28670,#28671,#28672,#28673,#28674,#28675,#28676,#28677,
#28678,#28679,#28680,#28681,#28682,#28683,#28684,#28685,#28686,#28687,#28688,
#28689,#28690,#28691,#28692,#28693,#28694,#28695,#28696,#28697,#28698,#28699,
#28700,#28701,#28702,#28703,#28704,#28705,#28706,#28707,#28708,#28709,#28710,
#28711,#28712,#28713,#28714,#28715,#28716,#28717,#28718,#28719,#28720,#28721,
#28722,#28723,#28724,#28725,#28726,#28727,#28728,#28729,#28730,#28731,#28732,
#28733,#28734,#28735,#28736,#28737,#28738,#28739,#28740,#28741,#28742,#28743,
#28744,#28745,#28746,#28747,#28748,#28749,#28750,#28751,#28752,#28753,#28754,
#28755,#28756,#28757,#28758,#28759,#28760,#28761,#28762,#28763,#28764,#28765,
#28766,#28767,#28768,#28769,#28770,#28771,#28772,#28773,#28774),(#28775,
#28776,#28777,#28778,#28779,#28780,#28781,#28782,#28783,#28784,#28785,#28786,
#28787,#28788,#28789,#28790,#28791,#28792,#28793,#28794,#28795,#28796,#28797,
#28798,#28799,#28800,#28801,#28802,#28803,#28804,#28805,#28806,#28807,#28808,
#28809,#28810,#28811,#28812,#28813,#28814,#28815,#28816,#28817,#28818,#28819,
#28820,#28821,#28822,#28823,#28824,#28825,#28826,#28827,#28828,#28829,#28830,
#28831,#28832,#28833,#28834,#28835,#28836,#28837,#28838,#28839,#28840,#28841,
#28842,#28843,#28844,#28845,#28846,#28847,#28848,#28849,#28850,#28851,#28852,
#28853,#28854,#28855,#28856,#28857,#28858,#28859,#28860,#28861,#28862,#28863,
#28864,#28865,#28866,#28867,#28868,#28869,#28870,#28871,#28872,#28873,#28874,
#28875,#28876,#28877,#28878,#28879,#28880,#28881,#28882,#28883,#28884,#28885,
#28886,#28887,#28888,#28889,#28890,#28891,#28892,#28893,#28894,#28895,#28896,
#28897,#28898,#28899,#28900,#28901,#28902,#28903,#28904,#28905,#28906,#28907,
#28908,#28909,#28910,#28911,#28912,#28913,#28914,#28915,#28916,#28917,#28918,
#28919,#28920),(#28921,#28922,#28923,#28924,#28925,#28926,#28927,#28928,
#28929,#28930,#28931,#28932,#28933,#28934,#28935,#28936,#28937,#28938,#28939,
#28940,#28941,#28942,#28943,#28944,#28945,#28946,#28947,#28948,#28949,#28950,
#28951,#28952,#28953,#28954,#28955,#28956,#28957,#28958,#28959,#28960,#28961,
#28962,#28963,#28964,#28965,#28966,#28967,#28968,#28969,#28970,#28971,#28972,
#28973,#28974,#28975,#28976,#28977,#28978,#28979,#28980,#28981,#28982,#28983,
#28984,#28985,#28986,#28987,#28988,#28989,#28990,#28991,#28992,#28993,#28994,
#28995,#28996,#28997,#28998,#28999,#29000,#29001,#29002,#29003,#29004,#29005,
#29006,#29007,#29008,#29009,#29010,#29011,#29012,#29013,#29014,#29015,#29016,
#29017,#29018,#29019,#29020,#29021,#29022,#29023,#29024,#29025,#29026,#29027,
#29028,#29029,#29030,#29031,#29032,#29033,#29034,#29035,#29036,#29037,#29038,
#29039,#29040,#29041,#29042,#29043,#29044,#29045,#29046,#29047,#29048,#29049,
#29050,#29051,#29052,#29053,#29054,#29055,#29056,#29057,#29058,#29059,#29060,
#29061,#29062,#29063,#29064,#29065,#29066),(#29067,#29068,#29069,#29070,
#29071,#29072,#29073,#29074,#29075,#29076,#29077,#29078,#29079,#29080,#29081,
#29082,#29083,#29084,#29085,#29086,#29087,#29088,#29089,#29090,#29091,#29092,
#29093,#29094,#29095,#29096,#29097,#29098,#29099,#29100,#29101,#29102,#29103,
#29104,#29105,#29106,#29107,#29108,#29109,#29110,#29111,#29112,#29113,#29114,
#29115,#29116,#29117,#29118,#29119,#29120,#29121,#29122,#29123,#29124,#29125,
#29126,#29127,#29128,#29129,#29130,#29131,#29132,#29133,#29134,#29135,#29136,
#29137,#29138,#29139,#29140,#29141,#29142,#29143,#29144,#29145,#29146,#29147,
#29148,#29149,#29150,#29151,#29152,#29153,#29154,#29155,#29156,#29157,#29158,
#29159,#29160,#29161,#29162,#29163,#29164,#29165,#29166,#29167,#29168,#29169,
#29170,#29171,#29172,#29173,#29174,#29175,#29176,#29177,#29178,#29179,#29180,
#29181,#29182,#29183,#29184,#29185,#29186,#29187,#29188,#29189,#29190,#29191,
#29192,#29193,#29194,#29195,#29196,#29197,#29198,#29199,#29200,#29201,#29202,
#29203,#29204,#29205,#29206,#29207,#29208,#29209,#29210,#29211,#29212)),
 .UNSPECIFIED.,.F.,.F.,.F.,(4,4),(4,1,1,1,1,1,1,1,1,1,1,1,1,1,1,1,1,1,1,
1,1,1,1,1,1,1,1,1,1,1,1,1,1,1,1,1,1,1,1,1,1,1,1,1,1,1,1,1,1,1,1,1,1,1,1,
1,1,1,1,1,1,1,1,1,1,1,1,1,1,1,1,1,1,1,1,1,1,1,1,1,1,1,1,1,1,1,1,1,1,1,1,
1,1,1,1,1,1,1,1,1,1,1,1,1,1,1,1,1,1,1,1,1,1,1,1,1,1,1,1,1,1,1,1,1,1,1,1,
1,1,1,1,1,1,1,1,1,1,1,1,1,1,1,1,4),(0.,0.0460148164544131),(8.31058692273977,
9.30711355020657,10.3036401776734,11.3001668051402,12.296693432607,13.2932200600738,
14.2897466875406,15.2862733150074,16.2827999424742,17.279326569941,18.2758531974078,
19.2723798248745,20.2689064523413,21.2654330798081,22.2619597072749,23.2584863347417,
24.2550129622085,25.2515395896753,26.2480662171421,27.2445928446089,28.2411194720757,
29.2376460995425,30.2341727270093,31.2306993544761,32.2272259819429,33.2237526094097,
34.2202792368765,35.2168058643433,36.2133324918101,37.2098591192769,38.2063857467437,
39.2029123742105,40.1994390016773,41.1959656291441,42.1924922566109,43.1890188840777,
44.1855455115445,45.1820721390113,46.1785987664781,47.1751253939449,48.1716520214117,
49.1681786488785,50.1647052763453,51.1612319038121,52.1577585312789,53.1542851587457,
54.1508117862125,55.1473384136793,56.1438650411461,57.1403916686129,58.1369182960797,
59.1334449235465,60.1299715510133,61.1264981784801,62.1230248059469,63.1195514334137,
64.1160780608805,65.1126046883473,66.1091313158141,67.1056579432809,68.1021845707477,
69.0987111982145,70.0952378256813,71.0917644531481,72.0882910806149,73.0848177080817,
74.0813443355485,75.0778709630153,76.0743975904821,77.0709242179488,78.0674508454156,
79.0639774728824,80.0605041003492,81.057030727816,82.0535573552828,83.0500839827496,
84.0466106102164,85.0431372376832,86.03966386515,87.0361904926168,88.0327171200836,
89.0292437475504,90.0257703750172,91.022297002484,92.0188236299508,93.0153502574176,
94.0118768848844,95.0084035123512,96.004930139818,97.0014567672848,97.9979833947516,
98.9945100222184,99.9910366496852,100.987563277152,101.984089904619,102.980616532086,
103.977143159552,104.973669787019,105.970196414486,106.966723041953,107.96324966942,
108.959776296886,109.956302924353,110.95282955182,111.949356179287,112.945882806754,
113.94240943422,114.938936061687,115.935462689154,116.931989316621,117.928515944088,
118.925042571554,119.921569199021,120.918095826488,121.914622453955,122.911149081422,
123.907675708888,124.904202336355,125.900728963822,126.897255591289,127.893782218756,
128.890308846222,129.886835473689,130.883362101156,131.879888728623,132.87641535609,
133.872941983556,134.869468611023,135.86599523849,136.862521865957,137.859048493424,
138.85557512089,139.852101748357,140.848628375824,141.845155003291,142.841681630758,
143.838208258224,144.834734885691,145.831261513158,146.827788140625,147.824314768092,
148.820841395558,149.817368023025,150.813894650492),.UNSPECIFIED.);
#115=B_SPLINE_SURFACE_WITH_KNOTS('',3,3,((#29504,#29505,#29506,#29507,#29508,
#29509,#29510,#29511,#29512,#29513,#29514,#29515,#29516,#29517,#29518,#29519,
#29520,#29521,#29522,#29523,#29524,#29525,#29526,#29527,#29528,#29529,#29530,
#29531,#29532,#29533,#29534,#29535,#29536,#29537,#29538,#29539,#29540,#29541,
#29542,#29543,#29544,#29545,#29546,#29547,#29548,#29549,#29550,#29551,#29552,
#29553,#29554,#29555,#29556,#29557,#29558,#29559,#29560,#29561,#29562,#29563,
#29564,#29565,#29566,#29567,#29568,#29569,#29570,#29571,#29572,#29573,#29574,
#29575,#29576,#29577,#29578,#29579,#29580,#29581,#29582,#29583,#29584,#29585,
#29586,#29587,#29588,#29589,#29590,#29591,#29592,#29593,#29594,#29595,#29596,
#29597,#29598,#29599,#29600,#29601,#29602,#29603,#29604,#29605,#29606,#29607,
#29608,#29609,#29610,#29611,#29612,#29613,#29614,#29615,#29616,#29617,#29618,
#29619,#29620,#29621,#29622,#29623,#29624,#29625,#29626,#29627,#29628,#29629,
#29630,#29631,#29632,#29633,#29634,#29635,#29636,#29637,#29638,#29639,#29640,
#29641,#29642,#29643,#29644,#29645,#29646,#29647,#29648,#29649),(#29650,
#29651,#29652,#29653,#29654,#29655,#29656,#29657,#29658,#29659,#29660,#29661,
#29662,#29663,#29664,#29665,#29666,#29667,#29668,#29669,#29670,#29671,#29672,
#29673,#29674,#29675,#29676,#29677,#29678,#29679,#29680,#29681,#29682,#29683,
#29684,#29685,#29686,#29687,#29688,#29689,#29690,#29691,#29692,#29693,#29694,
#29695,#29696,#29697,#29698,#29699,#29700,#29701,#29702,#29703,#29704,#29705,
#29706,#29707,#29708,#29709,#29710,#29711,#29712,#29713,#29714,#29715,#29716,
#29717,#29718,#29719,#29720,#29721,#29722,#29723,#29724,#29725,#29726,#29727,
#29728,#29729,#29730,#29731,#29732,#29733,#29734,#29735,#29736,#29737,#29738,
#29739,#29740,#29741,#29742,#29743,#29744,#29745,#29746,#29747,#29748,#29749,
#29750,#29751,#29752,#29753,#29754,#29755,#29756,#29757,#29758,#29759,#29760,
#29761,#29762,#29763,#29764,#29765,#29766,#29767,#29768,#29769,#29770,#29771,
#29772,#29773,#29774,#29775,#29776,#29777,#29778,#29779,#29780,#29781,#29782,
#29783,#29784,#29785,#29786,#29787,#29788,#29789,#29790,#29791,#29792,#29793,
#29794,#29795),(#29796,#29797,#29798,#29799,#29800,#29801,#29802,#29803,
#29804,#29805,#29806,#29807,#29808,#29809,#29810,#29811,#29812,#29813,#29814,
#29815,#29816,#29817,#29818,#29819,#29820,#29821,#29822,#29823,#29824,#29825,
#29826,#29827,#29828,#29829,#29830,#29831,#29832,#29833,#29834,#29835,#29836,
#29837,#29838,#29839,#29840,#29841,#29842,#29843,#29844,#29845,#29846,#29847,
#29848,#29849,#29850,#29851,#29852,#29853,#29854,#29855,#29856,#29857,#29858,
#29859,#29860,#29861,#29862,#29863,#29864,#29865,#29866,#29867,#29868,#29869,
#29870,#29871,#29872,#29873,#29874,#29875,#29876,#29877,#29878,#29879,#29880,
#29881,#29882,#29883,#29884,#29885,#29886,#29887,#29888,#29889,#29890,#29891,
#29892,#29893,#29894,#29895,#29896,#29897,#29898,#29899,#29900,#29901,#29902,
#29903,#29904,#29905,#29906,#29907,#29908,#29909,#29910,#29911,#29912,#29913,
#29914,#29915,#29916,#29917,#29918,#29919,#29920,#29921,#29922,#29923,#29924,
#29925,#29926,#29927,#29928,#29929,#29930,#29931,#29932,#29933,#29934,#29935,
#29936,#29937,#29938,#29939,#29940,#29941),(#29942,#29943,#29944,#29945,
#29946,#29947,#29948,#29949,#29950,#29951,#29952,#29953,#29954,#29955,#29956,
#29957,#29958,#29959,#29960,#29961,#29962,#29963,#29964,#29965,#29966,#29967,
#29968,#29969,#29970,#29971,#29972,#29973,#29974,#29975,#29976,#29977,#29978,
#29979,#29980,#29981,#29982,#29983,#29984,#29985,#29986,#29987,#29988,#29989,
#29990,#29991,#29992,#29993,#29994,#29995,#29996,#29997,#29998,#29999,#30000,
#30001,#30002,#30003,#30004,#30005,#30006,#30007,#30008,#30009,#30010,#30011,
#30012,#30013,#30014,#30015,#30016,#30017,#30018,#30019,#30020,#30021,#30022,
#30023,#30024,#30025,#30026,#30027,#30028,#30029,#30030,#30031,#30032,#30033,
#30034,#30035,#30036,#30037,#30038,#30039,#30040,#30041,#30042,#30043,#30044,
#30045,#30046,#30047,#30048,#30049,#30050,#30051,#30052,#30053,#30054,#30055,
#30056,#30057,#30058,#30059,#30060,#30061,#30062,#30063,#30064,#30065,#30066,
#30067,#30068,#30069,#30070,#30071,#30072,#30073,#30074,#30075,#30076,#30077,
#30078,#30079,#30080,#30081,#30082,#30083,#30084,#30085,#30086,#30087)),
 .UNSPECIFIED.,.F.,.F.,.F.,(4,4),(4,1,1,1,1,1,1,1,1,1,1,1,1,1,1,1,1,1,1,
1,1,1,1,1,1,1,1,1,1,1,1,1,1,1,1,1,1,1,1,1,1,1,1,1,1,1,1,1,1,1,1,1,1,1,1,
1,1,1,1,1,1,1,1,1,1,1,1,1,1,1,1,1,1,1,1,1,1,1,1,1,1,1,1,1,1,1,1,1,1,1,1,
1,1,1,1,1,1,1,1,1,1,1,1,1,1,1,1,1,1,1,1,1,1,1,1,1,1,1,1,1,1,1,1,1,1,1,1,
1,1,1,1,1,1,1,1,1,1,1,1,1,1,1,1,4),(0.,0.0460148164544131),(11.6154215191106,
12.6119481465774,13.6084747740442,14.605001401511,15.6015280289778,16.5980546564446,
17.5945812839114,18.5911079113782,19.587634538845,20.5841611663118,21.5806877937786,
22.5772144212454,23.5737410487122,24.570267676179,25.5667943036458,26.5633209311126,
27.5598475585794,28.5563741860462,29.552900813513,30.5494274409798,31.5459540684466,
32.5424806959134,33.5390073233802,34.535533950847,35.5320605783138,36.5285872057806,
37.5251138332474,38.5216404607142,39.518167088181,40.5146937156478,41.5112203431146,
42.5077469705814,43.5042735980482,44.500800225515,45.4973268529818,46.4938534804486,
47.4903801079154,48.4869067353822,49.483433362849,50.4799599903158,51.4764866177826,
52.4730132452493,53.4695398727161,54.4660665001829,55.4625931276497,56.4591197551165,
57.4556463825833,58.4521730100501,59.4486996375169,60.4452262649837,61.4417528924505,
62.4382795199173,63.4348061473841,64.4313327748509,65.4278594023177,66.4243860297845,
67.4209126572513,68.4174392847181,69.4139659121849,70.4104925396517,71.4070191671185,
72.4035457945853,73.4000724220521,74.3965990495189,75.3931256769857,76.3896523044525,
77.3861789319193,78.3827055593861,79.3792321868529,80.3757588143197,81.3722854417865,
82.3688120692533,83.3653386967201,84.3618653241869,85.3583919516537,86.3549185791205,
87.3514452065873,88.3479718340541,89.3444984615209,90.3410250889877,91.3375517164545,
92.3340783439213,93.3306049713881,94.3271315988549,95.3236582263217,96.3201848537885,
97.3167114812553,98.313238108722,99.3097647361889,100.306291363656,101.302817991122,
102.299344618589,103.295871246056,104.292397873523,105.28892450099,106.285451128456,
107.281977755923,108.27850438339,109.275031010857,110.271557638324,111.26808426579,
112.264610893257,113.261137520724,114.257664148191,115.254190775658,116.250717403124,
117.247244030591,118.243770658058,119.240297285525,120.236823912992,121.233350540458,
122.229877167925,123.226403795392,124.222930422859,125.219457050326,126.215983677792,
127.212510305259,128.209036932726,129.205563560193,130.20209018766,131.198616815126,
132.195143442593,133.19167007006,134.188196697527,135.184723324994,136.18124995246,
137.177776579927,138.174303207394,139.170829834861,140.167356462328,141.163883089794,
142.160409717261,143.156936344728,144.153462972195,145.149989599662,146.146516227128,
147.143042854595,148.139569482062,149.136096109529,150.132622736996,151.129149364462,
152.125675991929,153.122202619396,154.118729246863),.UNSPECIFIED.);
#116=B_SPLINE_SURFACE_WITH_KNOTS('',3,3,((#32297,#32298,#32299,#32300,#32301,
#32302,#32303,#32304,#32305,#32306,#32307,#32308,#32309,#32310,#32311,#32312,
#32313,#32314,#32315,#32316,#32317,#32318,#32319,#32320,#32321,#32322,#32323,
#32324,#32325,#32326,#32327,#32328,#32329,#32330,#32331,#32332,#32333,#32334,
#32335,#32336,#32337,#32338,#32339,#32340,#32341,#32342,#32343,#32344,#32345,
#32346,#32347,#32348,#32349,#32350,#32351,#32352,#32353,#32354,#32355,#32356,
#32357,#32358,#32359,#32360,#32361,#32362,#32363,#32364,#32365,#32366,#32367,
#32368,#32369,#32370,#32371,#32372,#32373,#32374,#32375,#32376,#32377,#32378,
#32379,#32380,#32381,#32382,#32383,#32384,#32385,#32386,#32387,#32388,#32389,
#32390,#32391,#32392,#32393,#32394,#32395,#32396,#32397,#32398,#32399,#32400,
#32401,#32402,#32403,#32404,#32405,#32406,#32407,#32408,#32409,#32410,#32411,
#32412,#32413,#32414,#32415,#32416,#32417,#32418,#32419,#32420,#32421,#32422,
#32423,#32424,#32425,#32426,#32427,#32428,#32429,#32430,#32431,#32432,#32433,
#32434,#32435,#32436,#32437,#32438,#32439,#32440,#32441,#32442,#32443,#32444,
#32445,#32446,#32447,#32448,#32449,#32450,#32451,#32452,#32453,#32454,#32455,
#32456,#32457,#32458,#32459,#32460,#32461,#32462,#32463,#32464,#32465,#32466,
#32467,#32468,#32469,#32470,#32471,#32472,#32473,#32474,#32475,#32476,#32477,
#32478),(#32479,#32480,#32481,#32482,#32483,#32484,#32485,#32486,#32487,
#32488,#32489,#32490,#32491,#32492,#32493,#32494,#32495,#32496,#32497,#32498,
#32499,#32500,#32501,#32502,#32503,#32504,#32505,#32506,#32507,#32508,#32509,
#32510,#32511,#32512,#32513,#32514,#32515,#32516,#32517,#32518,#32519,#32520,
#32521,#32522,#32523,#32524,#32525,#32526,#32527,#32528,#32529,#32530,#32531,
#32532,#32533,#32534,#32535,#32536,#32537,#32538,#32539,#32540,#32541,#32542,
#32543,#32544,#32545,#32546,#32547,#32548,#32549,#32550,#32551,#32552,#32553,
#32554,#32555,#32556,#32557,#32558,#32559,#32560,#32561,#32562,#32563,#32564,
#32565,#32566,#32567,#32568,#32569,#32570,#32571,#32572,#32573,#32574,#32575,
#32576,#32577,#32578,#32579,#32580,#32581,#32582,#32583,#32584,#32585,#32586,
#32587,#32588,#32589,#32590,#32591,#32592,#32593,#32594,#32595,#32596,#32597,
#32598,#32599,#32600,#32601,#32602,#32603,#32604,#32605,#32606,#32607,#32608,
#32609,#32610,#32611,#32612,#32613,#32614,#32615,#32616,#32617,#32618,#32619,
#32620,#32621,#32622,#32623,#32624,#32625,#32626,#32627,#32628,#32629,#32630,
#32631,#32632,#32633,#32634,#32635,#32636,#32637,#32638,#32639,#32640,#32641,
#32642,#32643,#32644,#32645,#32646,#32647,#32648,#32649,#32650,#32651,#32652,
#32653,#32654,#32655,#32656,#32657,#32658,#32659,#32660),(#32661,#32662,
#32663,#32664,#32665,#32666,#32667,#32668,#32669,#32670,#32671,#32672,#32673,
#32674,#32675,#32676,#32677,#32678,#32679,#32680,#32681,#32682,#32683,#32684,
#32685,#32686,#32687,#32688,#32689,#32690,#32691,#32692,#32693,#32694,#32695,
#32696,#32697,#32698,#32699,#32700,#32701,#32702,#32703,#32704,#32705,#32706,
#32707,#32708,#32709,#32710,#32711,#32712,#32713,#32714,#32715,#32716,#32717,
#32718,#32719,#32720,#32721,#32722,#32723,#32724,#32725,#32726,#32727,#32728,
#32729,#32730,#32731,#32732,#32733,#32734,#32735,#32736,#32737,#32738,#32739,
#32740,#32741,#32742,#32743,#32744,#32745,#32746,#32747,#32748,#32749,#32750,
#32751,#32752,#32753,#32754,#32755,#32756,#32757,#32758,#32759,#32760,#32761,
#32762,#32763,#32764,#32765,#32766,#32767,#32768,#32769,#32770,#32771,#32772,
#32773,#32774,#32775,#32776,#32777,#32778,#32779,#32780,#32781,#32782,#32783,
#32784,#32785,#32786,#32787,#32788,#32789,#32790,#32791,#32792,#32793,#32794,
#32795,#32796,#32797,#32798,#32799,#32800,#32801,#32802,#32803,#32804,#32805,
#32806,#32807,#32808,#32809,#32810,#32811,#32812,#32813,#32814,#32815,#32816,
#32817,#32818,#32819,#32820,#32821,#32822,#32823,#32824,#32825,#32826,#32827,
#32828,#32829,#32830,#32831,#32832,#32833,#32834,#32835,#32836,#32837,#32838,
#32839,#32840,#32841,#32842),(#32843,#32844,#32845,#32846,#32847,#32848,
#32849,#32850,#32851,#32852,#32853,#32854,#32855,#32856,#32857,#32858,#32859,
#32860,#32861,#32862,#32863,#32864,#32865,#32866,#32867,#32868,#32869,#32870,
#32871,#32872,#32873,#32874,#32875,#32876,#32877,#32878,#32879,#32880,#32881,
#32882,#32883,#32884,#32885,#32886,#32887,#32888,#32889,#32890,#32891,#32892,
#32893,#32894,#32895,#32896,#32897,#32898,#32899,#32900,#32901,#32902,#32903,
#32904,#32905,#32906,#32907,#32908,#32909,#32910,#32911,#32912,#32913,#32914,
#32915,#32916,#32917,#32918,#32919,#32920,#32921,#32922,#32923,#32924,#32925,
#32926,#32927,#32928,#32929,#32930,#32931,#32932,#32933,#32934,#32935,#32936,
#32937,#32938,#32939,#32940,#32941,#32942,#32943,#32944,#32945,#32946,#32947,
#32948,#32949,#32950,#32951,#32952,#32953,#32954,#32955,#32956,#32957,#32958,
#32959,#32960,#32961,#32962,#32963,#32964,#32965,#32966,#32967,#32968,#32969,
#32970,#32971,#32972,#32973,#32974,#32975,#32976,#32977,#32978,#32979,#32980,
#32981,#32982,#32983,#32984,#32985,#32986,#32987,#32988,#32989,#32990,#32991,
#32992,#32993,#32994,#32995,#32996,#32997,#32998,#32999,#33000,#33001,#33002,
#33003,#33004,#33005,#33006,#33007,#33008,#33009,#33010,#33011,#33012,#33013,
#33014,#33015,#33016,#33017,#33018,#33019,#33020,#33021,#33022,#33023,#33024)),
 .UNSPECIFIED.,.F.,.F.,.F.,(4,4),(4,1,1,1,1,1,1,1,1,1,1,1,1,1,1,1,1,1,1,
1,1,1,1,1,1,1,1,1,1,1,1,1,1,1,1,1,1,1,1,1,1,1,1,1,1,1,1,1,1,1,1,1,1,1,1,
1,1,1,1,1,1,1,1,1,1,1,1,1,1,1,1,1,1,1,1,1,1,1,1,1,1,1,1,1,1,1,1,1,1,1,1,
1,1,1,1,1,1,1,1,1,1,1,1,1,1,1,1,1,1,1,1,1,1,1,1,1,1,1,1,1,1,1,1,1,1,1,1,
1,1,1,1,1,1,1,1,1,1,1,1,1,1,1,1,1,1,1,1,1,1,1,1,1,1,1,1,1,1,1,1,1,1,1,1,
1,1,1,1,1,1,1,1,1,1,1,1,1,1,1,1,4),(0.,0.0460148164544131),(8.3105869227399,
9.3072753236828,10.3039637246257,11.3006521255686,12.2973405265115,13.2940289274544,
14.2907173283973,15.2874057293402,16.2840941302831,17.280782531226,18.2774709321689,
19.2741593331118,20.2708477340547,21.2675361349975,22.2642245359404,23.2609129368833,
24.2576013378262,25.2542897387691,26.250978139712,27.2476665406549,28.2443549415978,
29.2410433425407,30.2377317434836,31.2344201444265,32.2311085453694,33.2277969463123,
34.2244853472552,35.2211737481981,36.217862149141,37.2145505500839,38.2112389510268,
39.2079273519697,40.2046157529126,41.2013041538555,42.1979925547984,43.1946809557413,
44.1913693566841,45.188057757627,46.18474615857,47.1814345595128,48.1781229604557,
49.1748113613986,50.1714997623415,51.1681881632844,52.1648765642273,53.1615649651702,
54.1582533661131,55.154941767056,56.1516301679989,57.1483185689418,58.1450069698847,
59.1416953708276,60.1383837717705,61.1350721727134,62.1317605736563,63.1284489745992,
64.1251373755421,65.121825776485,66.1185141774279,67.1152025783708,68.1118909793137,
69.1085793802565,70.1052677811994,71.1019561821423,72.0986445830852,73.0953329840281,
74.092021384971,75.0887097859139,76.0853981868568,77.0820865877997,78.0787749887426,
79.0754633896855,80.0721517906284,81.0688401915713,82.0655285925142,83.0622169934571,
84.0589053944,85.0555937953429,86.0522821962858,87.0489705972287,88.0456589981716,
89.0423473991145,90.0390358000574,91.0357242010002,92.0324126019432,93.029101002886,
94.0257894038289,95.0224778047718,96.0191662057147,97.0158546066576,98.0125430076005,
99.0092314085434,100.005919809486,101.002608210429,101.999296611372,102.995985012315,
103.992673413258,104.989361814201,105.986050215144,106.982738616087,107.979427017029,
108.976115417972,109.972803818915,110.969492219858,111.966180620801,112.962869021744,
113.959557422687,114.95624582363,115.952934224573,116.949622625516,117.946311026458,
118.942999427401,119.939687828344,120.936376229287,121.93306463023,122.929753031173,
123.926441432116,124.923129833059,125.919818234002,126.916506634944,127.913195035887,
128.90988343683,129.906571837773,130.903260238716,131.899948639659,132.896637040602,
133.893325441545,134.890013842488,135.886702243431,136.883390644373,137.880079045316,
138.876767446259,139.873455847202,140.870144248145,141.866832649088,142.863521050031,
143.860209450974,144.856897851917,145.85358625286,146.850274653802,147.846963054745,
148.843651455688,149.840339856631,150.837028257574,151.833716658517,152.83040505946,
153.827093460403,154.823781861346,155.820470262288,156.817158663231,157.813847064174,
158.810535465117,159.80722386606,160.803912267003,161.800600667946,162.797289068889,
163.793977469832,164.790665870775,165.787354271717,166.78404267266,167.780731073603,
168.777419474546,169.774107875489,170.770796276432,171.767484677375,172.764173078318,
173.760861479261,174.757549880203,175.754238281146,176.750926682089,177.747615083032,
178.744303483975,179.740991884918,180.737680285861,181.734368686804,182.731057087747,
183.72774548869,184.724433889632,185.721122290575,186.717810691518),
 .UNSPECIFIED.);
#117=B_SPLINE_SURFACE_WITH_KNOTS('',3,3,((#33328,#33329,#33330,#33331,#33332,
#33333,#33334,#33335,#33336,#33337,#33338,#33339,#33340,#33341,#33342,#33343,
#33344,#33345,#33346,#33347,#33348,#33349,#33350,#33351,#33352,#33353,#33354,
#33355,#33356,#33357,#33358,#33359,#33360,#33361,#33362,#33363,#33364,#33365,
#33366,#33367,#33368,#33369,#33370,#33371,#33372,#33373,#33374,#33375,#33376,
#33377,#33378,#33379,#33380,#33381,#33382,#33383,#33384,#33385,#33386,#33387,
#33388,#33389,#33390,#33391,#33392,#33393,#33394,#33395,#33396,#33397,#33398,
#33399,#33400,#33401,#33402,#33403,#33404,#33405,#33406,#33407,#33408,#33409,
#33410,#33411,#33412,#33413,#33414,#33415,#33416,#33417,#33418,#33419,#33420,
#33421,#33422,#33423,#33424,#33425,#33426,#33427,#33428,#33429,#33430,#33431,
#33432,#33433,#33434,#33435,#33436,#33437,#33438,#33439,#33440,#33441,#33442,
#33443,#33444,#33445,#33446,#33447,#33448,#33449,#33450,#33451,#33452,#33453,
#33454,#33455,#33456,#33457,#33458,#33459,#33460,#33461,#33462,#33463,#33464,
#33465,#33466,#33467,#33468,#33469,#33470,#33471,#33472,#33473,#33474,#33475,
#33476,#33477,#33478,#33479,#33480,#33481,#33482,#33483,#33484,#33485,#33486,
#33487,#33488,#33489,#33490,#33491,#33492,#33493,#33494,#33495,#33496,#33497,
#33498,#33499,#33500,#33501,#33502,#33503,#33504,#33505,#33506,#33507,#33508,
#33509),(#33510,#33511,#33512,#33513,#33514,#33515,#33516,#33517,#33518,
#33519,#33520,#33521,#33522,#33523,#33524,#33525,#33526,#33527,#33528,#33529,
#33530,#33531,#33532,#33533,#33534,#33535,#33536,#33537,#33538,#33539,#33540,
#33541,#33542,#33543,#33544,#33545,#33546,#33547,#33548,#33549,#33550,#33551,
#33552,#33553,#33554,#33555,#33556,#33557,#33558,#33559,#33560,#33561,#33562,
#33563,#33564,#33565,#33566,#33567,#33568,#33569,#33570,#33571,#33572,#33573,
#33574,#33575,#33576,#33577,#33578,#33579,#33580,#33581,#33582,#33583,#33584,
#33585,#33586,#33587,#33588,#33589,#33590,#33591,#33592,#33593,#33594,#33595,
#33596,#33597,#33598,#33599,#33600,#33601,#33602,#33603,#33604,#33605,#33606,
#33607,#33608,#33609,#33610,#33611,#33612,#33613,#33614,#33615,#33616,#33617,
#33618,#33619,#33620,#33621,#33622,#33623,#33624,#33625,#33626,#33627,#33628,
#33629,#33630,#33631,#33632,#33633,#33634,#33635,#33636,#33637,#33638,#33639,
#33640,#33641,#33642,#33643,#33644,#33645,#33646,#33647,#33648,#33649,#33650,
#33651,#33652,#33653,#33654,#33655,#33656,#33657,#33658,#33659,#33660,#33661,
#33662,#33663,#33664,#33665,#33666,#33667,#33668,#33669,#33670,#33671,#33672,
#33673,#33674,#33675,#33676,#33677,#33678,#33679,#33680,#33681,#33682,#33683,
#33684,#33685,#33686,#33687,#33688,#33689,#33690,#33691),(#33692,#33693,
#33694,#33695,#33696,#33697,#33698,#33699,#33700,#33701,#33702,#33703,#33704,
#33705,#33706,#33707,#33708,#33709,#33710,#33711,#33712,#33713,#33714,#33715,
#33716,#33717,#33718,#33719,#33720,#33721,#33722,#33723,#33724,#33725,#33726,
#33727,#33728,#33729,#33730,#33731,#33732,#33733,#33734,#33735,#33736,#33737,
#33738,#33739,#33740,#33741,#33742,#33743,#33744,#33745,#33746,#33747,#33748,
#33749,#33750,#33751,#33752,#33753,#33754,#33755,#33756,#33757,#33758,#33759,
#33760,#33761,#33762,#33763,#33764,#33765,#33766,#33767,#33768,#33769,#33770,
#33771,#33772,#33773,#33774,#33775,#33776,#33777,#33778,#33779,#33780,#33781,
#33782,#33783,#33784,#33785,#33786,#33787,#33788,#33789,#33790,#33791,#33792,
#33793,#33794,#33795,#33796,#33797,#33798,#33799,#33800,#33801,#33802,#33803,
#33804,#33805,#33806,#33807,#33808,#33809,#33810,#33811,#33812,#33813,#33814,
#33815,#33816,#33817,#33818,#33819,#33820,#33821,#33822,#33823,#33824,#33825,
#33826,#33827,#33828,#33829,#33830,#33831,#33832,#33833,#33834,#33835,#33836,
#33837,#33838,#33839,#33840,#33841,#33842,#33843,#33844,#33845,#33846,#33847,
#33848,#33849,#33850,#33851,#33852,#33853,#33854,#33855,#33856,#33857,#33858,
#33859,#33860,#33861,#33862,#33863,#33864,#33865,#33866,#33867,#33868,#33869,
#33870,#33871,#33872,#33873),(#33874,#33875,#33876,#33877,#33878,#33879,
#33880,#33881,#33882,#33883,#33884,#33885,#33886,#33887,#33888,#33889,#33890,
#33891,#33892,#33893,#33894,#33895,#33896,#33897,#33898,#33899,#33900,#33901,
#33902,#33903,#33904,#33905,#33906,#33907,#33908,#33909,#33910,#33911,#33912,
#33913,#33914,#33915,#33916,#33917,#33918,#33919,#33920,#33921,#33922,#33923,
#33924,#33925,#33926,#33927,#33928,#33929,#33930,#33931,#33932,#33933,#33934,
#33935,#33936,#33937,#33938,#33939,#33940,#33941,#33942,#33943,#33944,#33945,
#33946,#33947,#33948,#33949,#33950,#33951,#33952,#33953,#33954,#33955,#33956,
#33957,#33958,#33959,#33960,#33961,#33962,#33963,#33964,#33965,#33966,#33967,
#33968,#33969,#33970,#33971,#33972,#33973,#33974,#33975,#33976,#33977,#33978,
#33979,#33980,#33981,#33982,#33983,#33984,#33985,#33986,#33987,#33988,#33989,
#33990,#33991,#33992,#33993,#33994,#33995,#33996,#33997,#33998,#33999,#34000,
#34001,#34002,#34003,#34004,#34005,#34006,#34007,#34008,#34009,#34010,#34011,
#34012,#34013,#34014,#34015,#34016,#34017,#34018,#34019,#34020,#34021,#34022,
#34023,#34024,#34025,#34026,#34027,#34028,#34029,#34030,#34031,#34032,#34033,
#34034,#34035,#34036,#34037,#34038,#34039,#34040,#34041,#34042,#34043,#34044,
#34045,#34046,#34047,#34048,#34049,#34050,#34051,#34052,#34053,#34054,#34055)),
 .UNSPECIFIED.,.F.,.F.,.F.,(4,4),(4,1,1,1,1,1,1,1,1,1,1,1,1,1,1,1,1,1,1,
1,1,1,1,1,1,1,1,1,1,1,1,1,1,1,1,1,1,1,1,1,1,1,1,1,1,1,1,1,1,1,1,1,1,1,1,
1,1,1,1,1,1,1,1,1,1,1,1,1,1,1,1,1,1,1,1,1,1,1,1,1,1,1,1,1,1,1,1,1,1,1,1,
1,1,1,1,1,1,1,1,1,1,1,1,1,1,1,1,1,1,1,1,1,1,1,1,1,1,1,1,1,1,1,1,1,1,1,1,
1,1,1,1,1,1,1,1,1,1,1,1,1,1,1,1,1,1,1,1,1,1,1,1,1,1,1,1,1,1,1,1,1,1,1,1,
1,1,1,1,1,1,1,1,1,1,1,1,1,1,1,1,4),(0.,0.0460148164544131),(11.6154215191108,
12.6121099200537,13.6087983209966,14.6054867219395,15.6021751228824,16.5988635238253,
17.5955519247682,18.592240325711,19.5889287266539,20.5856171275968,21.5823055285397,
22.5789939294826,23.5756823304255,24.5723707313684,25.5690591323113,26.5657475332542,
27.5624359341971,28.55912433514,29.5558127360829,30.5525011370258,31.5491895379687,
32.5458779389116,33.5425663398545,34.5392547407974,35.5359431417403,36.5326315426832,
37.5293199436261,38.526008344569,39.5226967455119,40.5193851464548,41.5160735473976,
42.5127619483405,43.5094503492834,44.5061387502263,45.5028271511692,46.4995155521121,
47.496203953055,48.4928923539979,49.4895807549408,50.4862691558837,51.4829575568266,
52.4796459577695,53.4763343587124,54.4730227596553,55.4697111605982,56.4663995615411,
57.463087962484,58.4597763634269,59.4564647643698,60.4531531653127,61.4498415662556,
62.4465299671985,63.4432183681413,64.4399067690842,65.4365951700271,66.43328357097,
67.4299719719129,68.4266603728558,69.4233487737987,70.4200371747416,71.4167255756845,
72.4134139766274,73.4101023775703,74.4067907785132,75.4034791794561,76.400167580399,
77.3968559813419,78.3935443822848,79.3902327832277,80.3869211841706,81.3836095851135,
82.3802979860564,83.3769863869992,84.3736747879422,85.3703631888851,86.3670515898279,
87.3637399907708,88.3604283917137,89.3571167926566,90.3538051935995,91.3504935945424,
92.3471819954853,93.3438703964282,94.3405587973711,95.337247198314,96.3339355992569,
97.3306240001998,98.3273124011427,99.3240008020856,100.320689203028,101.317377603971,
102.314066004914,103.310754405857,104.3074428068,105.304131207743,106.300819608686,
107.297508009629,108.294196410572,109.290884811515,110.287573212457,111.2842616134,
112.280950014343,113.277638415286,114.274326816229,115.271015217172,116.267703618115,
117.264392019058,118.261080420001,119.257768820943,120.254457221886,121.251145622829,
122.247834023772,123.244522424715,124.241210825658,125.237899226601,126.234587627544,
127.231276028487,128.22796442943,129.224652830372,130.221341231315,131.218029632258,
132.214718033201,133.211406434144,134.208094835087,135.20478323603,136.201471636973,
137.198160037916,138.194848438859,139.191536839801,140.188225240744,141.184913641687,
142.18160204263,143.178290443573,144.174978844516,145.171667245459,146.168355646402,
147.165044047345,148.161732448287,149.15842084923,150.155109250173,151.151797651116,
152.148486052059,153.145174453002,154.141862853945,155.138551254888,156.135239655831,
157.131928056774,158.128616457716,159.125304858659,160.121993259602,161.118681660545,
162.115370061488,163.112058462431,164.108746863374,165.105435264317,166.10212366526,
167.098812066202,168.095500467145,169.092188868088,170.088877269031,171.085565669974,
172.082254070917,173.07894247186,174.075630872803,175.072319273746,176.069007674689,
177.065696075631,178.062384476574,179.059072877517,180.05576127846,181.052449679403,
182.049138080346,183.045826481289,184.042514882232,185.039203283175,186.035891684118,
187.03258008506,188.029268486003,189.025956886946,190.022645287889),
 .UNSPECIFIED.);
#118=B_SPLINE_SURFACE_WITH_KNOTS('',3,3,((#35741,#35742,#35743,#35744,#35745,
#35746,#35747,#35748,#35749,#35750,#35751,#35752,#35753,#35754,#35755,#35756,
#35757,#35758,#35759,#35760,#35761,#35762,#35763,#35764,#35765,#35766,#35767,
#35768,#35769,#35770,#35771,#35772,#35773,#35774,#35775,#35776,#35777,#35778,
#35779,#35780,#35781,#35782,#35783,#35784,#35785,#35786,#35787,#35788,#35789,
#35790,#35791,#35792,#35793,#35794,#35795,#35796,#35797,#35798,#35799,#35800,
#35801,#35802,#35803,#35804,#35805,#35806,#35807,#35808,#35809,#35810,#35811,
#35812,#35813,#35814,#35815,#35816,#35817,#35818,#35819,#35820,#35821,#35822,
#35823,#35824,#35825,#35826,#35827,#35828,#35829,#35830,#35831,#35832,#35833,
#35834,#35835,#35836,#35837,#35838,#35839,#35840,#35841,#35842,#35843,#35844,
#35845,#35846,#35847,#35848,#35849,#35850,#35851,#35852,#35853,#35854),
(#35855,#35856,#35857,#35858,#35859,#35860,#35861,#35862,#35863,#35864,
#35865,#35866,#35867,#35868,#35869,#35870,#35871,#35872,#35873,#35874,#35875,
#35876,#35877,#35878,#35879,#35880,#35881,#35882,#35883,#35884,#35885,#35886,
#35887,#35888,#35889,#35890,#35891,#35892,#35893,#35894,#35895,#35896,#35897,
#35898,#35899,#35900,#35901,#35902,#35903,#35904,#35905,#35906,#35907,#35908,
#35909,#35910,#35911,#35912,#35913,#35914,#35915,#35916,#35917,#35918,#35919,
#35920,#35921,#35922,#35923,#35924,#35925,#35926,#35927,#35928,#35929,#35930,
#35931,#35932,#35933,#35934,#35935,#35936,#35937,#35938,#35939,#35940,#35941,
#35942,#35943,#35944,#35945,#35946,#35947,#35948,#35949,#35950,#35951,#35952,
#35953,#35954,#35955,#35956,#35957,#35958,#35959,#35960,#35961,#35962,#35963,
#35964,#35965,#35966,#35967,#35968),(#35969,#35970,#35971,#35972,#35973,
#35974,#35975,#35976,#35977,#35978,#35979,#35980,#35981,#35982,#35983,#35984,
#35985,#35986,#35987,#35988,#35989,#35990,#35991,#35992,#35993,#35994,#35995,
#35996,#35997,#35998,#35999,#36000,#36001,#36002,#36003,#36004,#36005,#36006,
#36007,#36008,#36009,#36010,#36011,#36012,#36013,#36014,#36015,#36016,#36017,
#36018,#36019,#36020,#36021,#36022,#36023,#36024,#36025,#36026,#36027,#36028,
#36029,#36030,#36031,#36032,#36033,#36034,#36035,#36036,#36037,#36038,#36039,
#36040,#36041,#36042,#36043,#36044,#36045,#36046,#36047,#36048,#36049,#36050,
#36051,#36052,#36053,#36054,#36055,#36056,#36057,#36058,#36059,#36060,#36061,
#36062,#36063,#36064,#36065,#36066,#36067,#36068,#36069,#36070,#36071,#36072,
#36073,#36074,#36075,#36076,#36077,#36078,#36079,#36080,#36081,#36082),
(#36083,#36084,#36085,#36086,#36087,#36088,#36089,#36090,#36091,#36092,
#36093,#36094,#36095,#36096,#36097,#36098,#36099,#36100,#36101,#36102,#36103,
#36104,#36105,#36106,#36107,#36108,#36109,#36110,#36111,#36112,#36113,#36114,
#36115,#36116,#36117,#36118,#36119,#36120,#36121,#36122,#36123,#36124,#36125,
#36126,#36127,#36128,#36129,#36130,#36131,#36132,#36133,#36134,#36135,#36136,
#36137,#36138,#36139,#36140,#36141,#36142,#36143,#36144,#36145,#36146,#36147,
#36148,#36149,#36150,#36151,#36152,#36153,#36154,#36155,#36156,#36157,#36158,
#36159,#36160,#36161,#36162,#36163,#36164,#36165,#36166,#36167,#36168,#36169,
#36170,#36171,#36172,#36173,#36174,#36175,#36176,#36177,#36178,#36179,#36180,
#36181,#36182,#36183,#36184,#36185,#36186,#36187,#36188,#36189,#36190,#36191,
#36192,#36193,#36194,#36195,#36196)),.UNSPECIFIED.,.F.,.F.,.F.,(4,4),(4,
1,1,1,1,1,1,1,1,1,1,1,1,1,1,1,1,1,1,1,1,1,1,1,1,1,1,1,1,1,1,1,1,1,1,1,1,
1,1,1,1,1,1,1,1,1,1,1,1,1,1,1,1,1,1,1,1,1,1,1,1,1,1,1,1,1,1,1,1,1,1,1,1,
1,1,1,1,1,1,1,1,1,1,1,1,1,1,1,1,1,1,1,1,1,1,1,1,1,1,1,1,1,1,1,1,1,1,1,1,
1,1,4),(0.,0.0296469363228873),(8.30626835282484,9.30418594221277,10.3021035316007,
11.3000211209886,12.2979387103766,13.2958562997645,14.2937738891524,15.2916914785404,
16.2896090679283,17.2875266573163,18.2854442467042,19.2833618360921,20.2812794254801,
21.279197014868,22.2771146042559,23.2750321936439,24.2729497830318,25.2708673724197,
26.2687849618077,27.2667025511956,28.2646201405835,29.2625377299715,30.2604553193594,
31.2583729087473,32.2562904981353,33.2542080875232,34.2521256769111,35.2500432662991,
36.247960855687,37.245878445075,38.2437960344629,39.2417136238508,40.2396312132388,
41.2375488026267,42.2354663920146,43.2333839814026,44.2313015707905,45.2292191601784,
46.2271367495664,47.2250543389543,48.2229719283422,49.2208895177302,50.2188071071181,
51.216724696506,52.214642285894,53.2125598752819,54.2104774646699,55.2083950540578,
56.2063126434457,57.2042302328337,58.2021478222216,59.2000654116095,60.1979830009975,
61.1959005903854,62.1938181797733,63.1917357691613,64.1896533585492,65.1875709479371,
66.1854885373251,67.183406126713,68.1813237161009,69.1792413054889,70.1771588948768,
71.1750764842647,72.1729940736527,73.1709116630406,74.1688292524286,75.1667468418165,
76.1646644312044,77.1625820205924,78.1604996099803,79.1584171993682,80.1563347887562,
81.1542523781441,82.152169967532,83.15008755692,84.1480051463079,85.1459227356958,
86.1438403250838,87.1417579144717,88.1396755038596,89.1375930932476,90.1355106826355,
91.1334282720235,92.1313458614114,93.1292634507993,94.1271810401873,95.1250986295752,
96.1230162189631,97.1209338083511,98.118851397739,99.1167689871269,100.114686576515,
101.112604165903,102.110521755291,103.108439344679,104.106356934067,105.104274523455,
106.102192112842,107.10010970223,108.098027291618,109.095944881006,110.093862470394,
111.091780059782,112.08969764917,113.087615238558,114.085532827946,115.083450417334,
116.081368006722,117.07928559611,118.077203185498,119.075120774886),
 .UNSPECIFIED.);
#119=B_SPLINE_SURFACE_WITH_KNOTS('',3,3,((#36473,#36474,#36475,#36476,#36477,
#36478,#36479,#36480,#36481,#36482,#36483,#36484,#36485,#36486,#36487,#36488,
#36489,#36490,#36491,#36492,#36493,#36494,#36495,#36496,#36497,#36498,#36499,
#36500,#36501,#36502,#36503,#36504,#36505,#36506,#36507,#36508,#36509,#36510,
#36511,#36512,#36513,#36514,#36515,#36516,#36517,#36518,#36519,#36520,#36521,
#36522,#36523,#36524,#36525,#36526,#36527,#36528,#36529,#36530,#36531,#36532,
#36533,#36534,#36535,#36536,#36537,#36538,#36539,#36540,#36541,#36542,#36543,
#36544,#36545,#36546,#36547,#36548,#36549,#36550,#36551,#36552,#36553,#36554,
#36555,#36556,#36557,#36558,#36559,#36560,#36561,#36562,#36563,#36564,#36565,
#36566,#36567,#36568,#36569,#36570,#36571,#36572,#36573,#36574,#36575,#36576,
#36577,#36578,#36579,#36580,#36581,#36582,#36583,#36584,#36585,#36586),
(#36587,#36588,#36589,#36590,#36591,#36592,#36593,#36594,#36595,#36596,
#36597,#36598,#36599,#36600,#36601,#36602,#36603,#36604,#36605,#36606,#36607,
#36608,#36609,#36610,#36611,#36612,#36613,#36614,#36615,#36616,#36617,#36618,
#36619,#36620,#36621,#36622,#36623,#36624,#36625,#36626,#36627,#36628,#36629,
#36630,#36631,#36632,#36633,#36634,#36635,#36636,#36637,#36638,#36639,#36640,
#36641,#36642,#36643,#36644,#36645,#36646,#36647,#36648,#36649,#36650,#36651,
#36652,#36653,#36654,#36655,#36656,#36657,#36658,#36659,#36660,#36661,#36662,
#36663,#36664,#36665,#36666,#36667,#36668,#36669,#36670,#36671,#36672,#36673,
#36674,#36675,#36676,#36677,#36678,#36679,#36680,#36681,#36682,#36683,#36684,
#36685,#36686,#36687,#36688,#36689,#36690,#36691,#36692,#36693,#36694,#36695,
#36696,#36697,#36698,#36699,#36700),(#36701,#36702,#36703,#36704,#36705,
#36706,#36707,#36708,#36709,#36710,#36711,#36712,#36713,#36714,#36715,#36716,
#36717,#36718,#36719,#36720,#36721,#36722,#36723,#36724,#36725,#36726,#36727,
#36728,#36729,#36730,#36731,#36732,#36733,#36734,#36735,#36736,#36737,#36738,
#36739,#36740,#36741,#36742,#36743,#36744,#36745,#36746,#36747,#36748,#36749,
#36750,#36751,#36752,#36753,#36754,#36755,#36756,#36757,#36758,#36759,#36760,
#36761,#36762,#36763,#36764,#36765,#36766,#36767,#36768,#36769,#36770,#36771,
#36772,#36773,#36774,#36775,#36776,#36777,#36778,#36779,#36780,#36781,#36782,
#36783,#36784,#36785,#36786,#36787,#36788,#36789,#36790,#36791,#36792,#36793,
#36794,#36795,#36796,#36797,#36798,#36799,#36800,#36801,#36802,#36803,#36804,
#36805,#36806,#36807,#36808,#36809,#36810,#36811,#36812,#36813,#36814),
(#36815,#36816,#36817,#36818,#36819,#36820,#36821,#36822,#36823,#36824,
#36825,#36826,#36827,#36828,#36829,#36830,#36831,#36832,#36833,#36834,#36835,
#36836,#36837,#36838,#36839,#36840,#36841,#36842,#36843,#36844,#36845,#36846,
#36847,#36848,#36849,#36850,#36851,#36852,#36853,#36854,#36855,#36856,#36857,
#36858,#36859,#36860,#36861,#36862,#36863,#36864,#36865,#36866,#36867,#36868,
#36869,#36870,#36871,#36872,#36873,#36874,#36875,#36876,#36877,#36878,#36879,
#36880,#36881,#36882,#36883,#36884,#36885,#36886,#36887,#36888,#36889,#36890,
#36891,#36892,#36893,#36894,#36895,#36896,#36897,#36898,#36899,#36900,#36901,
#36902,#36903,#36904,#36905,#36906,#36907,#36908,#36909,#36910,#36911,#36912,
#36913,#36914,#36915,#36916,#36917,#36918,#36919,#36920,#36921,#36922,#36923,
#36924,#36925,#36926,#36927,#36928)),.UNSPECIFIED.,.F.,.F.,.F.,(4,4),(4,
1,1,1,1,1,1,1,1,1,1,1,1,1,1,1,1,1,1,1,1,1,1,1,1,1,1,1,1,1,1,1,1,1,1,1,1,
1,1,1,1,1,1,1,1,1,1,1,1,1,1,1,1,1,1,1,1,1,1,1,1,1,1,1,1,1,1,1,1,1,1,1,1,
1,1,1,1,1,1,1,1,1,1,1,1,1,1,1,1,1,1,1,1,1,1,1,1,1,1,1,1,1,1,1,1,1,1,1,1,
1,1,4),(0.,0.0296469363228873),(11.6151336144495,12.6130512038375,13.6109687932254,
14.6088863826133,15.6068039720013,16.6047215613892,17.6026391507771,18.6005567401651,
19.598474329553,20.5963919189409,21.5943095083289,22.5922270977168,23.5901446871048,
24.5880622764927,25.5859798658806,26.5838974552686,27.5818150446565,28.5797326340444,
29.5776502234324,30.5755678128203,31.5734854022082,32.5714029915962,33.5693205809841,
34.567238170372,35.56515575976,36.5630733491479,37.5609909385358,38.5589085279238,
39.5568261173117,40.5547437066997,41.5526612960876,42.5505788854755,43.5484964748635,
44.5464140642514,45.5443316536393,46.5422492430273,47.5401668324152,48.5380844218031,
49.5360020111911,50.533919600579,51.5318371899669,52.5297547793549,53.5276723687428,
54.5255899581308,55.5235075475187,56.5214251369066,57.5193427262946,58.5172603156825,
59.5151779050704,60.5130954944584,61.5110130838463,62.5089306732342,63.5068482626222,
64.5047658520101,65.502683441398,66.500601030786,67.4985186201739,68.4964362095618,
69.4943537989498,70.4922713883377,71.4901889777257,72.4881065671136,73.4860241565015,
74.4839417458895,75.4818593352774,76.4797769246653,77.4776945140533,78.4756121034412,
79.4735296928291,80.4714472822171,81.469364871605,82.4672824609929,83.4652000503809,
84.4631176397688,85.4610352291567,86.4589528185447,87.4568704079326,88.4547879973206,
89.4527055867085,90.4506231760964,91.4485407654844,92.4464583548723,93.4443759442602,
94.4422935336482,95.4402111230361,96.438128712424,97.436046301812,98.4339638911999,
99.4318814805878,100.429799069976,101.427716659364,102.425634248752,103.42355183814,
104.421469427528,105.419387016915,106.417304606303,107.415222195691,108.413139785079,
109.411057374467,110.408974963855,111.406892553243,112.404810142631,113.402727732019,
114.400645321407,115.398562910795,116.396480500183,117.394398089571,118.392315678959,
119.390233268347,120.388150857734,121.386068447122,122.38398603651),
 .UNSPECIFIED.);
#120=B_SPLINE_CURVE_WITH_KNOTS('',3,(#20379,#20380,#20381,#20382),
 .UNSPECIFIED.,.F.,.F.,(4,4),(-0.0159210516924088,0.),.UNSPECIFIED.);
#121=B_SPLINE_CURVE_WITH_KNOTS('',3,(#20385,#20386,#20387,#20388),
 .UNSPECIFIED.,.F.,.F.,(4,4),(-0.0159210527656447,0.),.UNSPECIFIED.);
#122=B_SPLINE_CURVE_WITH_KNOTS('',3,(#20391,#20392,#20393,#20394),
 .UNSPECIFIED.,.F.,.F.,(4,4),(-0.0159210517190927,0.),.UNSPECIFIED.);
#123=B_SPLINE_CURVE_WITH_KNOTS('',3,(#20397,#20398,#20399,#20400),
 .UNSPECIFIED.,.F.,.F.,(4,4),(-0.0159210527692958,0.),.UNSPECIFIED.);
#124=B_SPLINE_CURVE_WITH_KNOTS('',3,(#20440,#20441,#20442,#20443),
 .UNSPECIFIED.,.F.,.F.,(4,4),(-0.0698067370947057,0.),.UNSPECIFIED.);
#125=B_SPLINE_CURVE_WITH_KNOTS('',3,(#20446,#20447,#20448,#20449),
 .UNSPECIFIED.,.F.,.F.,(4,4),(-0.0698065886608642,0.),.UNSPECIFIED.);
#126=B_SPLINE_CURVE_WITH_KNOTS('',3,(#20455,#20456,#20457,#20458),
 .UNSPECIFIED.,.F.,.F.,(4,4),(-0.0698067370949415,0.),.UNSPECIFIED.);
#127=B_SPLINE_CURVE_WITH_KNOTS('',3,(#20461,#20462,#20463,#20464),
 .UNSPECIFIED.,.F.,.F.,(4,4),(-0.0698065886603473,0.),.UNSPECIFIED.);
#128=B_SPLINE_CURVE_WITH_KNOTS('',3,(#21070,#21071,#21072,#21073),
 .UNSPECIFIED.,.F.,.F.,(4,4),(0.278246822734795,0.803148805386867),
 .UNSPECIFIED.);
#129=B_SPLINE_CURVE_WITH_KNOTS('',3,(#21075,#21076,#21077,#21078,#21079,
#21080),.UNSPECIFIED.,.F.,.F.,(4,2,4),(-0.339290689117984,-0.30404357328347,
-0.268796457448958),.UNSPECIFIED.);
#130=B_SPLINE_CURVE_WITH_KNOTS('',3,(#21081,#21082,#21083,#21084),
 .UNSPECIFIED.,.F.,.F.,(4,4),(-0.803148805386868,-0.278246822734795),
 .UNSPECIFIED.);
#131=B_SPLINE_CURVE_WITH_KNOTS('',3,(#21159,#21160,#21161,#21162),
 .UNSPECIFIED.,.F.,.F.,(4,4),(3.41983947632457,3.94474145897665),
 .UNSPECIFIED.);
#132=B_SPLINE_CURVE_WITH_KNOTS('',3,(#21164,#21165,#21166,#21167,#21168,
#21169),.UNSPECIFIED.,.F.,.F.,(4,2,4),(-0.33929068911798,-0.304043573283469,
-0.268796457448958),.UNSPECIFIED.);
#133=B_SPLINE_CURVE_WITH_KNOTS('',3,(#21170,#21171,#21172,#21173),
 .UNSPECIFIED.,.F.,.F.,(4,4),(2.33844384820293,2.86334583085503),
 .UNSPECIFIED.);
#134=B_SPLINE_CURVE_WITH_KNOTS('',3,(#21209,#21210,#21211,#21212,#21213,
#21214),.UNSPECIFIED.,.F.,.F.,(4,2,4),(0.268796457448958,0.30404357328347,
0.339290689117984),.UNSPECIFIED.);
#135=B_SPLINE_CURVE_WITH_KNOTS('',3,(#21239,#21240,#21241,#21242),
 .UNSPECIFIED.,.F.,.F.,(4,4),(0.278246822734795,0.803148805386868),
 .UNSPECIFIED.);
#136=B_SPLINE_CURVE_WITH_KNOTS('',3,(#21259,#21260,#21261,#21262),
 .UNSPECIFIED.,.F.,.F.,(4,4),(-0.803148805386867,-0.278246822734795),
 .UNSPECIFIED.);
#137=B_SPLINE_CURVE_WITH_KNOTS('',3,(#21296,#21297,#21298,#21299),
 .UNSPECIFIED.,.F.,.F.,(4,4),(0.268796457448958,0.304043573283469),
 .UNSPECIFIED.);
#138=B_SPLINE_CURVE_WITH_KNOTS('',3,(#21300,#21301,#21302,#21303),
 .UNSPECIFIED.,.F.,.F.,(4,4),(0.304043573283469,0.33929068911798),
 .UNSPECIFIED.);
#139=B_SPLINE_CURVE_WITH_KNOTS('',3,(#21326,#21327,#21328,#21329),
 .UNSPECIFIED.,.F.,.F.,(4,4),(-2.86334583085503,-2.33844384820293),
 .UNSPECIFIED.);
#140=B_SPLINE_CURVE_WITH_KNOTS('',3,(#21346,#21347,#21348,#21349),
 .UNSPECIFIED.,.F.,.F.,(4,4),(-3.94474145897665,-3.41983947632457),
 .UNSPECIFIED.);
#141=B_SPLINE_CURVE_WITH_KNOTS('',3,(#21804,#21805,#21806,#21807,#21808,
#21809,#21810,#21811,#21812,#21813),.UNSPECIFIED.,.F.,.F.,(4,3,3,4),(-4.09299088010945,
-3.9782854001501,-2.98371405011257,-2.08103247056473),.UNSPECIFIED.);
#142=B_SPLINE_CURVE_WITH_KNOTS('',3,(#21816,#21817,#21818,#21819,#21820,
#21821,#21822),.UNSPECIFIED.,.F.,.F.,(4,3,4),(0.,0.994571350037526,1.12963424404512),
 .UNSPECIFIED.);
#143=B_SPLINE_CURVE_WITH_KNOTS('',3,(#21827,#21828,#21829,#21830,#21831,
#21832,#21833,#21834,#21835,#21836,#21837,#21838,#21839,#21840,#21841,#21842,
#21843,#21844,#21845,#21846,#21847,#21848),.UNSPECIFIED.,.F.,.F.,(4,3,3,
3,3,3,3,4),(-10.376176187289,-9.94571350037525,-8.95114215033773,-7.9565708003002,
-6.96199945026268,-5.96742810022515,-4.97285675018763,-4.09299088010945),
 .UNSPECIFIED.);
#144=B_SPLINE_CURVE_WITH_KNOTS('',3,(#21849,#21850,#21851,#21852,#21853,
#21854,#21855,#21856,#21857,#21858,#21859,#21860,#21861,#21862,#21863,#21864,
#21865,#21866,#21867,#21868,#21869,#21870),.UNSPECIFIED.,.F.,.F.,(4,3,3,
3,3,3,3,4),(1.12963424404512,1.98914270007505,2.98371405011257,3.9782854001501,
4.97285675018762,5.96742810022515,6.96199945026267,7.4128195512247),
 .UNSPECIFIED.);
#145=B_SPLINE_CURVE_WITH_KNOTS('',3,(#21875,#21876,#21877,#21878,#21879,
#21880,#21881,#21882,#21883,#21884,#21885,#21886,#21887,#21888,#21889,#21890,
#21891,#21892,#21893,#21894,#21895,#21896),.UNSPECIFIED.,.F.,.F.,(4,3,3,
3,3,3,3,4),(-16.6593614944686,-15.9131416006004,-14.9185702505629,-13.9239989005253,
-12.9294275504878,-11.9348562004503,-10.9402848504128,-10.376176187289),
 .UNSPECIFIED.);
#146=B_SPLINE_CURVE_WITH_KNOTS('',3,(#21897,#21898,#21899,#21900,#21901,
#21902,#21903,#21904,#21905,#21906,#21907,#21908,#21909,#21910,#21911,#21912,
#21913,#21914,#21915,#21916,#21917,#21918),.UNSPECIFIED.,.F.,.F.,(4,3,3,
3,3,3,3,4),(7.4128195512247,7.9565708003002,8.95114215033773,9.94571350037526,
10.9402848504128,11.9348562004503,12.9294275504878,13.6960048584043),
 .UNSPECIFIED.);
#147=B_SPLINE_CURVE_WITH_KNOTS('',3,(#21923,#21924,#21925,#21926,#21927,
#21928,#21929,#21930,#21931,#21932,#21933,#21934,#21935,#21936,#21937,#21938,
#21939,#21940,#21941,#21942,#21943,#21944,#21945,#21946,#21947),
 .UNSPECIFIED.,.F.,.F.,(4,3,3,3,3,3,3,3,4),(-22.9425468016482,-22.8751410508631,
-21.8805697008255,-20.885998350788,-19.8914270007505,-18.896855650713,-17.9022843006754,
-16.9077129506379,-16.6593614944686),.UNSPECIFIED.);
#148=B_SPLINE_CURVE_WITH_KNOTS('',3,(#21948,#21949,#21950,#21951,#21952,
#21953,#21954,#21955,#21956,#21957,#21958,#21959,#21960,#21961,#21962,#21963,
#21964,#21965,#21966,#21967,#21968,#21969,#21970,#21971,#21972),
 .UNSPECIFIED.,.F.,.F.,(4,3,3,3,3,3,3,3,4),(13.6960048584043,13.9239989005254,
14.9185702505629,15.9131416006004,16.9077129506379,17.9022843006755,18.896855650713,
19.8914270007505,19.9791901655839),.UNSPECIFIED.);
#149=B_SPLINE_CURVE_WITH_KNOTS('',3,(#21977,#21978,#21979,#21980,#21981,
#21982,#21983,#21984,#21985,#21986,#21987,#21988,#21989,#21990,#21991,#21992,
#21993,#21994,#21995,#21996,#21997,#21998),.UNSPECIFIED.,.F.,.F.,(4,3,3,
3,3,3,3,4),(-29.2257321088278,-28.8425691510882,-27.8479978010507,-26.8534264510132,
-25.8588551009757,-24.8642837509381,-23.8697124009006,-22.9425468016482),
 .UNSPECIFIED.);
#150=B_SPLINE_CURVE_WITH_KNOTS('',3,(#21999,#22000,#22001,#22002,#22003,
#22004,#22005,#22006,#22007,#22008,#22009,#22010,#22011,#22012,#22013,#22014,
#22015,#22016,#22017,#22018,#22019,#22020),.UNSPECIFIED.,.F.,.F.,(4,3,3,
3,3,3,3,4),(19.9791901655839,20.885998350788,21.8805697008255,22.8751410508631,
23.8697124009006,24.8642837509381,25.8588551009756,26.2623754727635),
 .UNSPECIFIED.);
#151=B_SPLINE_CURVE_WITH_KNOTS('',3,(#22025,#22026,#22027,#22028,#22029,
#22030,#22031,#22032,#22033,#22034,#22035,#22036,#22037,#22038,#22039,#22040,
#22041,#22042,#22043,#22044,#22045,#22046),.UNSPECIFIED.,.F.,.F.,(4,3,3,
3,3,3,3,4),(-35.5089174160074,-34.8099972513134,-33.8154259012759,-32.8208545512383,
-31.8262832012008,-30.8317118511633,-29.8371405011258,-29.2257321088278),
 .UNSPECIFIED.);
#152=B_SPLINE_CURVE_WITH_KNOTS('',3,(#22047,#22048,#22049,#22050,#22051,
#22052,#22053,#22054,#22055,#22056,#22057,#22058,#22059,#22060,#22061,#22062,
#22063,#22064,#22065,#22066,#22067,#22068),.UNSPECIFIED.,.F.,.F.,(4,3,3,
3,3,3,3,4),(26.2623754727635,26.8534264510132,27.8479978010507,28.8425691510882,
29.8371405011258,30.8317118511633,31.8262832012008,32.545560779943),
 .UNSPECIFIED.);
#153=B_SPLINE_CURVE_WITH_KNOTS('',3,(#22073,#22074,#22075,#22076,#22077,
#22078,#22079,#22080,#22081,#22082,#22083,#22084,#22085,#22086,#22087,#22088,
#22089,#22090,#22091,#22092,#22093,#22094,#22095,#22096,#22097),
 .UNSPECIFIED.,.F.,.F.,(4,3,3,3,3,3,3,3,4),(-41.792102723187,-41.771996701576,
-40.7774253515385,-39.782854001501,-38.7882826514635,-37.7937113014259,
-36.7991399513884,-35.8045686013509,-35.5089174160074),.UNSPECIFIED.);
#154=B_SPLINE_CURVE_WITH_KNOTS('',3,(#22098,#22099,#22100,#22101,#22102,
#22103,#22104,#22105,#22106,#22107,#22108,#22109,#22110,#22111,#22112,#22113,
#22114,#22115,#22116,#22117,#22118,#22119,#22120,#22121,#22122),
 .UNSPECIFIED.,.F.,.F.,(4,3,3,3,3,3,3,3,4),(32.545560779943,32.8208545512383,
33.8154259012759,34.8099972513134,35.8045686013509,36.7991399513884,37.7937113014259,
38.7882826514634,38.8287460871226),.UNSPECIFIED.);
#155=B_SPLINE_CURVE_WITH_KNOTS('',3,(#22127,#22128,#22129,#22130,#22131,
#22132,#22133,#22134,#22135,#22136,#22137,#22138,#22139,#22140,#22141,#22142,
#22143,#22144,#22145,#22146,#22147,#22148),.UNSPECIFIED.,.F.,.F.,(4,3,3,
3,3,3,3,4),(-48.0752880303666,-47.7394248018012,-46.7448534517637,-45.7502821017261,
-44.7557107516886,-43.7611394016511,-42.7665680516136,-41.792102723187),
 .UNSPECIFIED.);
#156=B_SPLINE_CURVE_WITH_KNOTS('',3,(#22149,#22150,#22151,#22152,#22153,
#22154,#22155,#22156,#22157,#22158,#22159,#22160,#22161,#22162,#22163,#22164,
#22165,#22166,#22167,#22168,#22169,#22170),.UNSPECIFIED.,.F.,.F.,(4,3,3,
3,3,3,3,4),(38.8287460871226,39.782854001501,40.7774253515385,41.771996701576,
42.7665680516136,43.7611394016511,44.7557107516886,45.1119313943022),
 .UNSPECIFIED.);
#157=B_SPLINE_CURVE_WITH_KNOTS('',3,(#22175,#22176,#22177,#22178,#22179,
#22180,#22181,#22182,#22183,#22184,#22185,#22186,#22187,#22188,#22189,#22190,
#22191,#22192,#22193,#22194,#22195,#22196),.UNSPECIFIED.,.F.,.F.,(4,3,3,
3,3,3,3,4),(-54.3584733375462,-53.7068529020263,-52.7122815519888,-51.7177102019513,
-50.7231388519138,-49.7285675018762,-48.7339961518387,-48.0752880303666),
 .UNSPECIFIED.);
#158=B_SPLINE_CURVE_WITH_KNOTS('',3,(#22197,#22198,#22199,#22200,#22201,
#22202,#22203,#22204,#22205,#22206,#22207,#22208,#22209,#22210,#22211,#22212,
#22213,#22214,#22215,#22216,#22217,#22218),.UNSPECIFIED.,.F.,.F.,(4,3,3,
3,3,3,3,4),(45.1119313943022,45.7502821017262,46.7448534517637,47.7394248018012,
48.7339961518387,49.7285675018763,50.7231388519138,51.3951167014818),
 .UNSPECIFIED.);
#159=B_SPLINE_CURVE_WITH_KNOTS('',3,(#22223,#22224,#22225,#22226,#22227,
#22228,#22229,#22230,#22231,#22232,#22233,#22234,#22235,#22236,#22237,#22238,
#22239,#22240,#22241,#22242,#22243,#22244),.UNSPECIFIED.,.F.,.F.,(4,3,3,
3,3,3,3,4),(-60.6416586447258,-59.6742810022515,-58.679709652214,-57.6851383021764,
-56.6905669521389,-55.6959956021014,-54.7014242520639,-54.3584733375462),
 .UNSPECIFIED.);
#160=B_SPLINE_CURVE_WITH_KNOTS('',3,(#22245,#22246,#22247,#22248,#22249,
#22250,#22251,#22252,#22253,#22254,#22255,#22256,#22257,#22258,#22259,#22260,
#22261,#22262,#22263,#22264,#22265,#22266),.UNSPECIFIED.,.F.,.F.,(4,3,3,
3,3,3,3,4),(51.3951167014818,51.7177102019513,52.7122815519888,53.7068529020263,
54.7014242520639,55.6959956021014,56.6905669521389,57.6783020086614),
 .UNSPECIFIED.);
#161=B_SPLINE_CURVE_WITH_KNOTS('',3,(#22271,#22272,#22273,#22274,#22275,
#22276,#22277,#22278,#22279,#22280,#22281,#22282,#22283,#22284,#22285,#22286,
#22287,#22288,#22289,#22290,#22291,#22292,#22293,#22294,#22295),
 .UNSPECIFIED.,.F.,.F.,(4,3,3,3,3,3,3,3,4),(-66.9248439519054,-66.6362804525142,
-65.6417091024766,-64.6471377524391,-63.6525664024016,-62.6579950523641,
-61.6634237023265,-60.668852352289,-60.6416586447258),.UNSPECIFIED.);
#162=B_SPLINE_CURVE_WITH_KNOTS('',3,(#22296,#22297,#22298,#22299,#22300,
#22301,#22302,#22303,#22304,#22305,#22306,#22307,#22308,#22309,#22310,#22311,
#22312,#22313,#22314,#22315,#22316,#22317,#22318,#22319,#22320),
 .UNSPECIFIED.,.F.,.F.,(4,3,3,3,3,3,3,3,4),(57.6783020086614,57.6851383021765,
58.679709652214,59.6742810022515,60.668852352289,61.6634237023265,62.6579950523641,
63.6525664024016,63.961487315841),.UNSPECIFIED.);
#163=B_SPLINE_CURVE_WITH_KNOTS('',3,(#22325,#22326,#22327,#22328,#22329,
#22330,#22331,#22332,#22333,#22334,#22335,#22336,#22337,#22338,#22339,#22340,
#22341,#22342,#22343,#22344,#22345,#22346),.UNSPECIFIED.,.F.,.F.,(4,3,3,
3,3,3,3,4),(-73.2080292590849,-72.6037085527393,-71.6091372027018,-70.6145658526643,
-69.6199945026267,-68.6254231525892,-67.6308518025517,-66.9248439519054),
 .UNSPECIFIED.);
#164=B_SPLINE_CURVE_WITH_KNOTS('',3,(#22347,#22348,#22349,#22350,#22351,
#22352,#22353,#22354,#22355,#22356,#22357,#22358,#22359,#22360,#22361,#22362,
#22363,#22364,#22365,#22366,#22367,#22368),.UNSPECIFIED.,.F.,.F.,(4,3,3,
3,3,3,3,4),(63.961487315841,64.6471377524391,65.6417091024766,66.6362804525142,
67.6308518025517,68.6254231525892,69.6199945026268,70.2446726230206),
 .UNSPECIFIED.);
#165=B_SPLINE_CURVE_WITH_KNOTS('',3,(#22373,#22374,#22375,#22376,#22377,
#22378,#22379,#22380,#22381,#22382,#22383,#22384,#22385,#22386,#22387,#22388,
#22389,#22390,#22391,#22392,#22393,#22394),.UNSPECIFIED.,.F.,.F.,(4,3,3,
3,3,3,3,4),(-79.4912145662645,-78.5711366529645,-77.5765653029269,-76.5819939528894,
-75.5874226028519,-74.5928512528144,-73.5982799027768,-73.2080292590849),
 .UNSPECIFIED.);
#166=B_SPLINE_CURVE_WITH_KNOTS('',3,(#22395,#22396,#22397,#22398,#22399,
#22400,#22401,#22402,#22403,#22404,#22405,#22406,#22407,#22408,#22409,#22410,
#22411,#22412,#22413,#22414,#22415,#22416),.UNSPECIFIED.,.F.,.F.,(4,3,3,
3,3,3,3,4),(70.2446726230206,70.6145658526643,71.6091372027018,72.6037085527393,
73.5982799027769,74.5928512528144,75.5874226028519,76.5278579302002),
 .UNSPECIFIED.);
#167=B_SPLINE_CURVE_WITH_KNOTS('',3,(#22421,#22422,#22423,#22424,#22425,
#22426,#22427,#22428,#22429,#22430,#22431,#22432,#22433,#22434,#22435,#22436,
#22437,#22438,#22439,#22440,#22441,#22442,#22443,#22444,#22445),
 .UNSPECIFIED.,.F.,.F.,(4,3,3,3,3,3,3,3,4),(-85.7743998734441,-85.5331361032271,
-84.5385647531896,-83.5439934031521,-82.5494220531146,-81.554850703077,
-80.5602793530395,-79.565708003002,-79.4912145662645),.UNSPECIFIED.);
#168=B_SPLINE_CURVE_WITH_KNOTS('',3,(#22446,#22447,#22448,#22449,#22450,
#22451,#22452,#22453,#22454,#22455,#22456,#22457,#22458,#22459,#22460,#22461,
#22462,#22463,#22464,#22465,#22466,#22467,#22468,#22469,#22470),
 .UNSPECIFIED.,.F.,.F.,(4,3,3,3,3,3,3,3,4),(76.5278579302002,76.5819939528894,
77.576565302927,78.5711366529645,79.565708003002,80.5602793530395,81.5548507030771,
82.5494220531146,82.8110432373798),.UNSPECIFIED.);
#169=B_SPLINE_CURVE_WITH_KNOTS('',3,(#22475,#22476,#22477,#22478,#22479,
#22480,#22481,#22482,#22483,#22484,#22485,#22486,#22487,#22488,#22489,#22490,
#22491,#22492,#22493,#22494,#22495,#22496),.UNSPECIFIED.,.F.,.F.,(4,3,3,
3,3,3,3,4),(-92.0575851806237,-91.5005642034523,-90.5059928534148,-89.5114215033772,
-88.5168501533397,-87.5222788033022,-86.5277074532647,-85.7743998734441),
 .UNSPECIFIED.);
#170=B_SPLINE_CURVE_WITH_KNOTS('',3,(#22497,#22498,#22499,#22500,#22501,
#22502,#22503,#22504,#22505,#22506,#22507,#22508,#22509,#22510,#22511,#22512,
#22513,#22514,#22515,#22516,#22517,#22518),.UNSPECIFIED.,.F.,.F.,(4,3,3,
3,3,3,3,4),(82.8110432373798,83.5439934031521,84.5385647531896,85.5331361032272,
86.5277074532647,87.5222788033022,88.5168501533397,89.0942285445594),
 .UNSPECIFIED.);
#171=B_SPLINE_CURVE_WITH_KNOTS('',3,(#22523,#22524,#22525,#22526,#22527,
#22528,#22529,#22530,#22531,#22532,#22533,#22534,#22535,#22536,#22537,#22538,
#22539,#22540,#22541,#22542,#22543,#22544),.UNSPECIFIED.,.F.,.F.,(4,3,3,
3,3,3,3,4),(-98.3407704878033,-97.4679923036774,-96.4734209536399,-95.4788496036024,
-94.4842782535649,-93.4897069035273,-92.4951355534898,-92.0575851806237),
 .UNSPECIFIED.);
#172=B_SPLINE_CURVE_WITH_KNOTS('',3,(#22545,#22546,#22547,#22548,#22549,
#22550,#22551,#22552,#22553,#22554,#22555,#22556,#22557,#22558,#22559,#22560,
#22561,#22562,#22563,#22564,#22565,#22566),.UNSPECIFIED.,.F.,.F.,(4,3,3,
3,3,3,3,4),(89.0942285445594,89.5114215033772,90.5059928534148,91.5005642034523,
92.4951355534898,93.4897069035273,94.4842782535649,95.377413851739),
 .UNSPECIFIED.);
#173=B_SPLINE_CURVE_WITH_KNOTS('',3,(#22571,#22572,#22573,#22574,#22575,
#22576,#22577,#22578,#22579,#22580,#22581,#22582,#22583,#22584,#22585,#22586,
#22587,#22588,#22589,#22590,#22591,#22592,#22593,#22594,#22595),
 .UNSPECIFIED.,.F.,.F.,(4,3,3,3,3,3,3,3,4),(-104.623955794983,-104.42999175394,
-103.435420403903,-102.440849053865,-101.446277703828,-100.45170635379,
-99.4571350037525,-98.462563653715,-98.3407704878033),.UNSPECIFIED.);
#174=B_SPLINE_CURVE_WITH_KNOTS('',3,(#22596,#22597,#22598,#22599,#22600,
#22601,#22602,#22603,#22604,#22605,#22606,#22607,#22608,#22609,#22610,#22611,
#22612,#22613,#22614,#22615,#22616,#22617,#22618,#22619,#22620),
 .UNSPECIFIED.,.F.,.F.,(4,3,3,3,3,3,3,3,4),(95.377413851739,95.4788496036024,
96.4734209536399,97.4679923036774,98.462563653715,99.4571350037525,100.45170635379,
101.446277703828,101.660599158919),.UNSPECIFIED.);
#175=B_SPLINE_CURVE_WITH_KNOTS('',3,(#22625,#22626,#22627,#22628,#22629,
#22630,#22631,#22632,#22633,#22634,#22635,#22636,#22637,#22638,#22639,#22640,
#22641,#22642,#22643,#22644,#22645,#22646),.UNSPECIFIED.,.F.,.F.,(4,3,3,
3,3,3,3,4),(-110.907141102163,-110.397419854165,-109.402848504128,-108.40827715409,
-107.413705804053,-106.419134454015,-105.424563103978,-104.623955794983),
 .UNSPECIFIED.);
#176=B_SPLINE_CURVE_WITH_KNOTS('',3,(#22647,#22648,#22649,#22650,#22651,
#22652,#22653,#22654,#22655,#22656,#22657,#22658,#22659,#22660,#22661,#22662,
#22663,#22664,#22665,#22666,#22667,#22668),.UNSPECIFIED.,.F.,.F.,(4,3,3,
3,3,3,3,4),(101.660599158919,102.440849053865,103.435420403903,104.42999175394,
105.424563103978,106.419134454015,107.413705804053,107.943784466098),
 .UNSPECIFIED.);
#177=B_SPLINE_CURVE_WITH_KNOTS('',3,(#22673,#22674,#22675,#22676,#22677,
#22678,#22679,#22680,#22681,#22682,#22683,#22684,#22685,#22686,#22687,#22688,
#22689,#22690,#22691,#22692,#22693,#22694),.UNSPECIFIED.,.F.,.F.,(4,3,3,
3,3,3,3,4),(-117.190326409342,-116.36484795439,-115.370276604353,-114.375705254315,
-113.381133904278,-112.38656255424,-111.391991204203,-110.907141102163),
 .UNSPECIFIED.);
#178=B_SPLINE_CURVE_WITH_KNOTS('',3,(#22695,#22696,#22697,#22698,#22699,
#22700,#22701,#22702,#22703,#22704,#22705,#22706,#22707,#22708,#22709,#22710,
#22711,#22712,#22713,#22714,#22715,#22716),.UNSPECIFIED.,.F.,.F.,(4,3,3,
3,3,3,3,4),(107.943784466098,108.40827715409,109.402848504128,110.397419854165,
111.391991204203,112.38656255424,113.381133904278,114.226969773278),
 .UNSPECIFIED.);
#179=B_SPLINE_CURVE_WITH_KNOTS('',3,(#22721,#22722,#22723,#22724,#22725,
#22726,#22727,#22728,#22729,#22730,#22731,#22732,#22733,#22734,#22735,#22736,
#22737,#22738,#22739,#22740,#22741,#22742,#22743,#22744,#22745),
 .UNSPECIFIED.,.F.,.F.,(4,3,3,3,3,3,3,3,4),(-123.473511716522,-123.326847404653,
-122.332276054616,-121.337704704578,-120.343133354541,-119.348562004503,
-118.353990654465,-117.359419304428,-117.190326409342),.UNSPECIFIED.);
#180=B_SPLINE_CURVE_WITH_KNOTS('',3,(#22746,#22747,#22748,#22749,#22750,
#22751,#22752,#22753,#22754,#22755,#22756,#22757,#22758,#22759,#22760,#22761,
#22762,#22763,#22764,#22765,#22766,#22767,#22768,#22769,#22770),
 .UNSPECIFIED.,.F.,.F.,(4,3,3,3,3,3,3,3,4),(114.226969773278,114.375705254315,
115.370276604353,116.36484795439,117.359419304428,118.353990654465,119.348562004503,
120.343133354541,120.510155080457),.UNSPECIFIED.);
#181=B_SPLINE_CURVE_WITH_KNOTS('',3,(#22775,#22776,#22777,#22778,#22779,
#22780,#22781,#22782,#22783,#22784,#22785,#22786,#22787,#22788,#22789,#22790,
#22791,#22792,#22793,#22794,#22795,#22796),.UNSPECIFIED.,.F.,.F.,(4,3,3,
3,3,3,3,4),(-129.756697023701,-129.294275504878,-128.299704154841,-127.305132804803,
-126.310561454766,-125.315990104728,-124.321418754691,-123.473511716522),
 .UNSPECIFIED.);
#182=B_SPLINE_CURVE_WITH_KNOTS('',3,(#22797,#22798,#22799,#22800,#22801,
#22802,#22803,#22804,#22805,#22806,#22807,#22808,#22809,#22810,#22811,#22812,
#22813,#22814,#22815,#22816,#22817,#22818),.UNSPECIFIED.,.F.,.F.,(4,3,3,
3,3,3,3,4),(120.510155080457,121.337704704578,122.332276054616,123.326847404653,
124.321418754691,125.315990104728,126.310561454766,126.793340387637),
 .UNSPECIFIED.);
#183=B_SPLINE_CURVE_WITH_KNOTS('',3,(#22823,#22824,#22825,#22826,#22827,
#22828,#22829,#22830,#22831,#22832,#22833,#22834,#22835,#22836,#22837,#22838,
#22839,#22840,#22841,#22842,#22843,#22844),.UNSPECIFIED.,.F.,.F.,(4,3,3,
3,3,3,3,4),(-136.039882330881,-135.261703605103,-134.267132255066,-133.272560905028,
-132.277989554991,-131.283418204953,-130.288846854916,-129.756697023701),
 .UNSPECIFIED.);
#184=B_SPLINE_CURVE_WITH_KNOTS('',3,(#22845,#22846,#22847,#22848,#22849,
#22850,#22851,#22852,#22853,#22854,#22855,#22856,#22857,#22858,#22859,#22860,
#22861,#22862,#22863,#22864,#22865,#22866),.UNSPECIFIED.,.F.,.F.,(4,3,3,
3,3,3,3,4),(126.793340387637,127.305132804803,128.299704154841,129.294275504878,
130.288846854916,131.283418204953,132.277989554991,133.076525694817),
 .UNSPECIFIED.);
#185=B_SPLINE_CURVE_WITH_KNOTS('',3,(#22871,#22872,#22873,#22874,#22875,
#22876,#22877,#22878,#22879,#22880,#22881,#22882,#22883,#22884,#22885,#22886,
#22887,#22888,#22889,#22890,#22891,#22892,#22893,#22894,#22895),
 .UNSPECIFIED.,.F.,.F.,(4,3,3,3,3,3,3,3,4),(-142.32306763806,-142.223703055366,
-141.229131705329,-140.234560355291,-139.239989005253,-138.245417655216,
-137.250846305178,-136.256274955141,-136.039882330881),.UNSPECIFIED.);
#186=B_SPLINE_CURVE_WITH_KNOTS('',3,(#22896,#22897,#22898,#22899,#22900,
#22901,#22902,#22903,#22904,#22905,#22906,#22907,#22908,#22909,#22910,#22911,
#22912,#22913,#22914,#22915,#22916,#22917,#22918,#22919,#22920),
 .UNSPECIFIED.,.F.,.F.,(4,3,3,3,3,3,3,3,4),(133.076525694817,133.272560905028,
134.267132255066,135.261703605103,136.256274955141,137.250846305178,138.245417655216,
139.239989005254,139.359711001996),.UNSPECIFIED.);
#187=B_SPLINE_CURVE_WITH_KNOTS('',3,(#22925,#22926,#22927,#22928,#22929,
#22930,#22931,#22932,#22933,#22934,#22935,#22936,#22937,#22938,#22939,#22940,
#22941,#22942,#22943,#22944,#22945,#22946),.UNSPECIFIED.,.F.,.F.,(4,3,3,
3,3,3,3,4),(-148.60625294524,-148.191131155591,-147.196559805554,-146.201988455516,
-145.207417105479,-144.212845755441,-143.218274405404,-142.32306763806),
 .UNSPECIFIED.);
#188=B_SPLINE_CURVE_WITH_KNOTS('',3,(#22947,#22948,#22949,#22950,#22951,
#22952,#22953,#22954,#22955,#22956,#22957,#22958,#22959,#22960,#22961,#22962,
#22963,#22964,#22965,#22966,#22967,#22968),.UNSPECIFIED.,.F.,.F.,(4,3,3,
3,3,3,3,4),(139.359711001996,140.234560355291,141.229131705329,142.223703055366,
143.218274405404,144.212845755441,145.207417105479,145.642896309176),
 .UNSPECIFIED.);
#189=B_SPLINE_CURVE_WITH_KNOTS('',3,(#22973,#22974,#22975,#22976,#22977,
#22978,#22979,#22980,#22981,#22982,#22983,#22984,#22985,#22986,#22987,#22988,
#22989,#22990,#22991,#22992,#22993,#22994),.UNSPECIFIED.,.F.,.F.,(4,3,3,
3,3,3,3,4),(-154.88943825242,-154.158559255816,-153.163987905779,-152.169416555741,
-151.174845205704,-150.180273855666,-149.185702505629,-148.60625294524),
 .UNSPECIFIED.);
#190=B_SPLINE_CURVE_WITH_KNOTS('',3,(#22995,#22996,#22997,#22998,#22999,
#23000,#23001,#23002,#23003,#23004,#23005,#23006,#23007,#23008,#23009,#23010,
#23011,#23012,#23013,#23014,#23015,#23016),.UNSPECIFIED.,.F.,.F.,(4,3,3,
3,3,3,3,4),(145.642896309176,146.201988455516,147.196559805554,148.191131155591,
149.185702505629,150.180273855666,151.174845205704,151.926081616355),
 .UNSPECIFIED.);
#191=B_SPLINE_CURVE_WITH_KNOTS('',3,(#23021,#23022,#23023,#23024,#23025,
#23026,#23027,#23028,#23029,#23030,#23031,#23032,#23033,#23034,#23035,#23036,
#23037,#23038,#23039,#23040,#23041,#23042,#23043,#23044,#23045),
 .UNSPECIFIED.,.F.,.F.,(4,3,3,3,3,3,3,3,4),(-161.172623559599,-161.120558706079,
-160.125987356041,-159.131416006004,-158.136844655966,-157.142273305929,
-156.147701955891,-155.153130605854,-154.88943825242),.UNSPECIFIED.);
#192=B_SPLINE_CURVE_WITH_KNOTS('',3,(#23046,#23047,#23048,#23049,#23050,
#23051,#23052,#23053,#23054,#23055,#23056,#23057,#23058,#23059,#23060,#23061,
#23062,#23063,#23064,#23065,#23066,#23067,#23068,#23069,#23070),
 .UNSPECIFIED.,.F.,.F.,(4,3,3,3,3,3,3,3,4),(151.926081616355,152.169416555741,
153.163987905779,154.158559255816,155.153130605854,156.147701955891,157.142273305929,
158.136844655966,158.209266923535),.UNSPECIFIED.);
#193=B_SPLINE_CURVE_WITH_KNOTS('',3,(#23075,#23076,#23077,#23078,#23079,
#23080,#23081,#23082,#23083,#23084,#23085,#23086,#23087,#23088,#23089,#23090,
#23091,#23092,#23093,#23094,#23095,#23096),.UNSPECIFIED.,.F.,.F.,(4,3,3,
3,3,3,3,4),(-167.455808866779,-167.087986806304,-166.093415456267,-165.098844106229,
-164.104272756192,-163.109701406154,-162.115130056117,-161.172623559599),
 .UNSPECIFIED.);
#194=B_SPLINE_CURVE_WITH_KNOTS('',3,(#23097,#23098,#23099,#23100,#23101,
#23102,#23103,#23104,#23105,#23106,#23107,#23108,#23109,#23110,#23111,#23112,
#23113,#23114,#23115,#23116,#23117,#23118),.UNSPECIFIED.,.F.,.F.,(4,3,3,
3,3,3,3,4),(158.209266923535,159.131416006004,160.125987356042,161.120558706079,
162.115130056117,163.109701406154,164.104272756192,164.492452230714),
 .UNSPECIFIED.);
#195=B_SPLINE_CURVE_WITH_KNOTS('',3,(#23123,#23124,#23125,#23126,#23127,
#23128,#23129,#23130,#23131,#23132,#23133,#23134,#23135,#23136,#23137,#23138,
#23139,#23140,#23141,#23142,#23143,#23144),.UNSPECIFIED.,.F.,.F.,(4,3,3,
3,3,3,3,4),(-173.738994173958,-173.055414906529,-172.060843556492,-171.066272206454,
-170.071700856417,-169.077129506379,-168.082558156342,-167.455808866779),
 .UNSPECIFIED.);
#196=B_SPLINE_CURVE_WITH_KNOTS('',3,(#23145,#23146,#23147,#23148,#23149,
#23150,#23151,#23152,#23153,#23154,#23155,#23156,#23157,#23158,#23159,#23160,
#23161,#23162,#23163,#23164,#23165,#23166),.UNSPECIFIED.,.F.,.F.,(4,3,3,
3,3,3,3,4),(164.492452230714,165.098844106229,166.093415456267,167.087986806304,
168.082558156342,169.077129506379,170.071700856417,170.775637537894),
 .UNSPECIFIED.);
#197=B_SPLINE_CURVE_WITH_KNOTS('',3,(#23172,#23173,#23174,#23175,#23176,
#23177,#23178,#23179,#23180),.UNSPECIFIED.,.F.,.F.,(4,1,1,1,1,1,4),(179.070781254618,
179.697530544181,180.692101894219,181.686673244256,182.681244594294,183.675815944331,
184.578497523879),.UNSPECIFIED.);
#198=B_SPLINE_CURVE_WITH_KNOTS('',3,(#23183,#23184,#23185,#23186,#23187,
#23188,#23189,#23190),.UNSPECIFIED.,.F.,.F.,(4,1,1,1,1,4),(179.070781254618,
179.361415923179,180.355987273216,181.350558623254,182.345129973291,183.339701323329),
 .UNSPECIFIED.);
#199=B_SPLINE_CURVE_WITH_KNOTS('',3,(#23195,#23196,#23197,#23198,#23199,
#23200,#23201,#23202,#23203,#23204),.UNSPECIFIED.,.F.,.F.,(4,1,1,1,1,1,
1,4),(172.787595947439,173.730102443956,174.724673793994,175.719245144031,
176.713816494069,177.708387844106,178.702959194144,179.070781254618),
 .UNSPECIFIED.);
#200=B_SPLINE_CURVE_WITH_KNOTS('',3,(#23205,#23206,#23207,#23208,#23209,
#23210,#23211,#23212,#23213,#23214),.UNSPECIFIED.,.F.,.F.,(4,1,1,1,1,1,
1,4),(172.787595947439,173.393987822954,174.388559172991,175.383130523029,
176.377701873066,177.372273223104,178.366844573141,179.070781254618),
 .UNSPECIFIED.);
#201=B_SPLINE_CURVE_WITH_KNOTS('',3,(#23219,#23220,#23221,#23222,#23223,
#23224,#23225,#23226,#23227,#23228,#23229),.UNSPECIFIED.,.F.,.F.,(4,1,1,
1,1,1,1,1,4),(166.504410640259,166.768102993693,167.762674343731,168.757245693769,
169.751817043806,170.746388393844,171.740959743881,172.735531093919,172.787595947439),
 .UNSPECIFIED.);
#202=B_SPLINE_CURVE_WITH_KNOTS('',3,(#23230,#23231,#23232,#23233,#23234,
#23235,#23236,#23237,#23238,#23239),.UNSPECIFIED.,.F.,.F.,(4,1,1,1,1,1,
1,4),(166.504410640259,167.426559722728,168.421131072766,169.415702422803,
170.410273772841,171.404845122878,172.399416472916,172.787595947439),
 .UNSPECIFIED.);
#203=B_SPLINE_CURVE_WITH_KNOTS('',3,(#23244,#23245,#23246,#23247,#23248,
#23249,#23250,#23251,#23252,#23253),.UNSPECIFIED.,.F.,.F.,(4,1,1,1,1,1,
1,4),(160.22122533308,160.800674893468,161.795246243506,162.789817593543,
163.784388943581,164.778960293618,165.773531643656,166.504410640259),
 .UNSPECIFIED.);
#204=B_SPLINE_CURVE_WITH_KNOTS('',3,(#23254,#23255,#23256,#23257,#23258,
#23259,#23260,#23261,#23262,#23263,#23264),.UNSPECIFIED.,.F.,.F.,(4,1,1,
1,1,1,1,1,4),(160.22122533308,160.464560272466,161.459131622503,162.453702972541,
163.448274322578,164.442845672616,165.437417022653,166.431988372691,166.504410640259),
 .UNSPECIFIED.);
#205=B_SPLINE_CURVE_WITH_KNOTS('',3,(#23269,#23270,#23271,#23272,#23273,
#23274,#23275,#23276,#23277,#23278),.UNSPECIFIED.,.F.,.F.,(4,1,1,1,1,1,
1,4),(153.9380400259,154.833246793243,155.827818143281,156.822389493318,
157.816960843356,158.811532193393,159.806103543431,160.22122533308),
 .UNSPECIFIED.);
#206=B_SPLINE_CURVE_WITH_KNOTS('',3,(#23279,#23280,#23281,#23282,#23283,
#23284,#23285,#23286,#23287,#23288),.UNSPECIFIED.,.F.,.F.,(4,1,1,1,1,1,
1,4),(153.9380400259,154.497132172241,155.491703522278,156.486274872316,
157.480846222353,158.475417572391,159.469988922428,160.22122533308),
 .UNSPECIFIED.);
#207=B_SPLINE_CURVE_WITH_KNOTS('',3,(#23293,#23294,#23295,#23296,#23297,
#23298,#23299,#23300,#23301,#23302,#23303),.UNSPECIFIED.,.F.,.F.,(4,1,1,
1,1,1,1,1,4),(147.65485471872,147.87124734298,148.865818693018,149.860390043056,
150.854961393093,151.849532743131,152.844104093168,153.838675443206,153.9380400259),
 .UNSPECIFIED.);
#208=B_SPLINE_CURVE_WITH_KNOTS('',3,(#23304,#23305,#23306,#23307,#23308,
#23309,#23310,#23311,#23312,#23313),.UNSPECIFIED.,.F.,.F.,(4,1,1,1,1,1,
1,4),(147.65485471872,148.529704072015,149.524275422053,150.51884677209,
151.513418122128,152.507989472165,153.502560822203,153.9380400259),
 .UNSPECIFIED.);
#209=B_SPLINE_CURVE_WITH_KNOTS('',3,(#23318,#23319,#23320,#23321,#23322,
#23323,#23324,#23325,#23326,#23327),.UNSPECIFIED.,.F.,.F.,(4,1,1,1,1,1,
1,4),(141.371669411541,141.903819242755,142.898390592793,143.89296194283,
144.887533292868,145.882104642905,146.876675992943,147.65485471872),
 .UNSPECIFIED.);
#210=B_SPLINE_CURVE_WITH_KNOTS('',3,(#23328,#23329,#23330,#23331,#23332,
#23333,#23334,#23335,#23336,#23337,#23338),.UNSPECIFIED.,.F.,.F.,(4,1,1,
1,1,1,1,1,4),(141.371669411541,141.567704621753,142.56227597179,143.556847321828,
144.551418671865,145.545990021903,146.54056137194,147.535132721978,147.65485471872),
 .UNSPECIFIED.);
#211=B_SPLINE_CURVE_WITH_KNOTS('',3,(#23343,#23344,#23345,#23346,#23347,
#23348,#23349,#23350,#23351,#23352),.UNSPECIFIED.,.F.,.F.,(4,1,1,1,1,1,
1,4),(135.088484104361,135.93639114253,136.930962492568,137.925533842605,
138.920105192643,139.91467654268,140.909247892718,141.371669411541),
 .UNSPECIFIED.);
#212=B_SPLINE_CURVE_WITH_KNOTS('',3,(#23353,#23354,#23355,#23356,#23357,
#23358,#23359,#23360,#23361,#23362),.UNSPECIFIED.,.F.,.F.,(4,1,1,1,1,1,
1,4),(135.088484104361,135.600276521528,136.594847871565,137.589419221603,
138.58399057164,139.578561921678,140.573133271715,141.371669411541),
 .UNSPECIFIED.);
#213=B_SPLINE_CURVE_WITH_KNOTS('',3,(#23367,#23368,#23369,#23370,#23371,
#23372,#23373,#23374,#23375,#23376,#23377),.UNSPECIFIED.,.F.,.F.,(4,1,1,
1,1,1,1,1,4),(128.805298797182,128.974391692268,129.968963042305,130.963534392343,
131.95810574238,132.952677092418,133.947248442455,134.941819792493,135.088484104361),
 .UNSPECIFIED.);
#214=B_SPLINE_CURVE_WITH_KNOTS('',3,(#23378,#23379,#23380,#23381,#23382,
#23383,#23384,#23385,#23386,#23387),.UNSPECIFIED.,.F.,.F.,(4,1,1,1,1,1,
1,4),(128.805298797182,129.632848421302,130.62741977134,131.621991121377,
132.616562471415,133.611133821453,134.60570517149,135.088484104361),
 .UNSPECIFIED.);
#215=B_SPLINE_CURVE_WITH_KNOTS('',3,(#23392,#23393,#23394,#23395,#23396,
#23397,#23398,#23399,#23400,#23401),.UNSPECIFIED.,.F.,.F.,(4,1,1,1,1,1,
1,4),(122.522113490002,123.006963592042,124.00153494208,124.996106292117,
125.990677642155,126.985248992192,127.97982034223,128.805298797182),
 .UNSPECIFIED.);
#216=B_SPLINE_CURVE_WITH_KNOTS('',3,(#23402,#23403,#23404,#23405,#23406,
#23407,#23408,#23409,#23410,#23411,#23412),.UNSPECIFIED.,.F.,.F.,(4,1,1,
1,1,1,1,1,4),(122.522113490002,122.67084897104,123.665420321077,124.659991671115,
125.654563021152,126.64913437119,127.643705721227,128.638277071265,128.805298797182),
 .UNSPECIFIED.);
#217=B_SPLINE_CURVE_WITH_KNOTS('',3,(#23417,#23418,#23419,#23420,#23421,
#23422,#23423,#23424,#23425,#23426),.UNSPECIFIED.,.F.,.F.,(4,1,1,1,1,1,
1,4),(116.238928182823,117.039535491817,118.034106841855,119.028678191892,
120.02324954193,121.017820891967,122.012392242005,122.522113490002),
 .UNSPECIFIED.);
#218=B_SPLINE_CURVE_WITH_KNOTS('',3,(#23427,#23428,#23429,#23430,#23431,
#23432,#23433,#23434,#23435,#23436),.UNSPECIFIED.,.F.,.F.,(4,1,1,1,1,1,
1,4),(116.238928182823,116.703420870815,117.697992220852,118.69256357089,
119.687134920927,120.681706270965,121.676277621002,122.522113490002),
 .UNSPECIFIED.);
#219=B_SPLINE_CURVE_WITH_KNOTS('',3,(#23441,#23442,#23443,#23444,#23445,
#23446,#23447,#23448,#23449,#23450,#23451),.UNSPECIFIED.,.F.,.F.,(4,1,1,
1,1,1,1,1,4),(109.955742875643,110.077536041555,111.072107391592,112.06667874163,
113.061250091667,114.055821441705,115.050392791742,116.04496414178,116.238928182823),
 .UNSPECIFIED.);
#220=B_SPLINE_CURVE_WITH_KNOTS('',3,(#23452,#23453,#23454,#23455,#23456,
#23457,#23458,#23459,#23460,#23461),.UNSPECIFIED.,.F.,.F.,(4,1,1,1,1,1,
1,4),(109.955742875643,110.735992770589,111.730564120627,112.725135470664,
113.719706820702,114.71427817074,115.708849520777,116.238928182823),
 .UNSPECIFIED.);
#221=B_SPLINE_CURVE_WITH_KNOTS('',3,(#23466,#23467,#23468,#23469,#23470,
#23471,#23472,#23473,#23474,#23475),.UNSPECIFIED.,.F.,.F.,(4,1,1,1,1,1,
1,4),(103.672557568463,104.110107941329,105.104679291367,106.099250641404,
107.093821991442,108.08839334148,109.082964691517,109.955742875643),
 .UNSPECIFIED.);
#222=B_SPLINE_CURVE_WITH_KNOTS('',3,(#23476,#23477,#23478,#23479,#23480,
#23481,#23482,#23483,#23484,#23485,#23486),.UNSPECIFIED.,.F.,.F.,(4,1,1,
1,1,1,1,1,4),(103.672557568463,103.773993320327,104.768564670364,105.763136020402,
106.757707370439,107.752278720477,108.746850070514,109.741421420552,109.955742875643),
 .UNSPECIFIED.);
#223=B_SPLINE_CURVE_WITH_KNOTS('',3,(#23491,#23492,#23493,#23494,#23495,
#23496,#23497,#23498,#23499,#23500),.UNSPECIFIED.,.F.,.F.,(4,1,1,1,1,1,
1,4),(97.3893722612837,98.1426798411043,99.1372511911418,100.131822541179,
101.126393891217,102.120965241254,103.115536591292,103.672557568463),
 .UNSPECIFIED.);
#224=B_SPLINE_CURVE_WITH_KNOTS('',3,(#23501,#23502,#23503,#23504,#23505,
#23506,#23507,#23508,#23509,#23510),.UNSPECIFIED.,.F.,.F.,(4,1,1,1,1,1,
1,4),(97.3893722612837,97.8065652201016,98.8011365701391,99.7957079201767,
100.790279270214,101.784850620252,102.779421970289,103.672557568463),
 .UNSPECIFIED.);
#225=B_SPLINE_CURVE_WITH_KNOTS('',3,(#23515,#23516,#23517,#23518,#23519,
#23520,#23521,#23522,#23523,#23524,#23525),.UNSPECIFIED.,.F.,.F.,(4,1,1,
1,1,1,1,1,4),(91.1061869541041,91.1806803908416,92.1752517408791,93.1698230909166,
94.1643944409542,95.1589657909917,96.1535371410292,97.1481084910667,97.3893722612837),
 .UNSPECIFIED.);
#226=B_SPLINE_CURVE_WITH_KNOTS('',3,(#23526,#23527,#23528,#23529,#23530,
#23531,#23532,#23533,#23534,#23535),.UNSPECIFIED.,.F.,.F.,(4,1,1,1,1,1,
1,4),(91.1061869541041,91.8391371198765,92.833708469914,93.8282798199515,
94.822851169989,95.8174225200266,96.8119938700641,97.3893722612837),
 .UNSPECIFIED.);
#227=B_SPLINE_CURVE_WITH_KNOTS('',3,(#23540,#23541,#23542,#23543,#23544,
#23545,#23546,#23547,#23548,#23549),.UNSPECIFIED.,.F.,.F.,(4,1,1,1,1,1,
1,4),(84.8230016469245,85.2132522906164,86.207823640654,87.2023949906915,
88.196966340729,89.1915376907665,90.1861090408041,91.1061869541041),
 .UNSPECIFIED.);
#228=B_SPLINE_CURVE_WITH_KNOTS('',3,(#23550,#23551,#23552,#23553,#23554,
#23555,#23556,#23557,#23558,#23559,#23560),.UNSPECIFIED.,.F.,.F.,(4,1,1,
1,1,1,1,1,4),(84.8230016469246,84.8771376696138,85.8717090196513,86.8662803696888,
87.8608517197264,88.8554230697639,89.8499944198014,90.8445657698389,91.1061869541041),
 .UNSPECIFIED.);
#229=B_SPLINE_CURVE_WITH_KNOTS('',3,(#23565,#23566,#23567,#23568,#23569,
#23570,#23571,#23572,#23573,#23574),.UNSPECIFIED.,.F.,.F.,(4,1,1,1,1,1,
1,4),(78.539816339745,79.2458241903913,80.2403955404288,81.2349668904663,
82.2295382405039,83.2241095905414,84.2186809405789,84.8230016469245),
 .UNSPECIFIED.);
#230=B_SPLINE_CURVE_WITH_KNOTS('',3,(#23575,#23576,#23577,#23578,#23579,
#23580,#23581,#23582,#23583,#23584),.UNSPECIFIED.,.F.,.F.,(4,1,1,1,1,1,
1,4),(78.539816339745,78.9097095693886,79.9042809194262,80.8988522694637,
81.8934236195012,82.8879949695387,83.8825663195763,84.8230016469246),
 .UNSPECIFIED.);
#231=B_SPLINE_CURVE_WITH_KNOTS('',3,(#23589,#23590,#23591,#23592,#23593,
#23594,#23595,#23596,#23597,#23598,#23599),.UNSPECIFIED.,.F.,.F.,(4,1,1,
1,1,1,1,1,4),(72.2566310325654,72.2838247401286,73.2783960901661,74.2729674402037,
75.2675387902412,76.2621101402787,77.2566814903162,78.2512528403538,78.539816339745),
 .UNSPECIFIED.);
#232=B_SPLINE_CURVE_WITH_KNOTS('',3,(#23600,#23601,#23602,#23603,#23604,
#23605,#23606,#23607,#23608,#23609),.UNSPECIFIED.,.F.,.F.,(4,1,1,1,1,1,
1,4),(72.2566310325654,72.9422814691635,73.936852819201,74.9314241692385,
75.9259955192761,76.9205668693136,77.9151382193511,78.539816339745),
 .UNSPECIFIED.);
#233=B_SPLINE_CURVE_WITH_KNOTS('',3,(#23614,#23615,#23616,#23617,#23618,
#23619,#23620,#23621,#23622,#23623),.UNSPECIFIED.,.F.,.F.,(4,1,1,1,1,1,
1,4),(65.9734457253857,66.3163966399035,67.310967989941,68.3055393399785,
69.300110690016,70.2946820400536,71.2892533900911,72.2566310325654),
 .UNSPECIFIED.);
#234=B_SPLINE_CURVE_WITH_KNOTS('',3,(#23624,#23625,#23626,#23627,#23628,
#23629,#23630,#23631,#23632,#23633,#23634),.UNSPECIFIED.,.F.,.F.,(4,1,1,
1,1,1,1,1,4),(65.9734457253857,65.9802820189008,66.9748533689383,67.9694247189759,
68.9639960690134,69.9585674190509,70.9531387690884,71.947710119126,72.2566310325654),
 .UNSPECIFIED.);
#235=B_SPLINE_CURVE_WITH_KNOTS('',3,(#23639,#23640,#23641,#23642,#23643,
#23644,#23645,#23646,#23647,#23648),.UNSPECIFIED.,.F.,.F.,(4,1,1,1,1,1,
1,4),(59.6902604182062,60.3489685396783,61.3435398897158,62.3381112397534,
63.3326825897909,64.3272539398284,65.3218252898659,65.9734457253857),
 .UNSPECIFIED.);
#236=B_SPLINE_CURVE_WITH_KNOTS('',3,(#23649,#23650,#23651,#23652,#23653,
#23654,#23655,#23656,#23657,#23658),.UNSPECIFIED.,.F.,.F.,(4,1,1,1,1,1,
1,4),(59.6902604182062,60.0128539186757,61.0074252687132,62.0019966187507,
62.9965679687882,63.9911393188258,64.9857106688633,65.9734457253857),
 .UNSPECIFIED.);
#237=B_SPLINE_CURVE_WITH_KNOTS('',3,(#23663,#23664,#23665,#23666,#23667,
#23668,#23669,#23670,#23671,#23672),.UNSPECIFIED.,.F.,.F.,(4,1,1,1,1,1,
1,4),(53.4070751110266,54.3815404394532,55.3761117894907,56.3706831395282,
57.3652544895657,58.3598258396033,59.3543971896408,59.6902604182062),
 .UNSPECIFIED.);
#238=B_SPLINE_CURVE_WITH_KNOTS('',3,(#23673,#23674,#23675,#23676,#23677,
#23678,#23679,#23680,#23681,#23682),.UNSPECIFIED.,.F.,.F.,(4,1,1,1,1,1,
1,4),(53.4070751110266,54.0454258184505,55.039997168488,56.0345685185256,
57.0291398685631,58.0237112186006,59.0182825686381,59.6902604182062),
 .UNSPECIFIED.);
#239=B_SPLINE_CURVE_WITH_KNOTS('',3,(#23687,#23688,#23689,#23690,#23691,
#23692,#23693,#23694,#23695,#23696,#23697),.UNSPECIFIED.,.F.,.F.,(4,1,1,
1,1,1,1,1,4),(47.123889803847,47.4195409891905,48.414112339228,49.4086836892655,
50.4032550393031,51.3978263893406,52.3923977393781,53.3869690894156,53.4070751110266),
 .UNSPECIFIED.);
#240=B_SPLINE_CURVE_WITH_KNOTS('',3,(#23698,#23699,#23700,#23701,#23702,
#23703,#23704,#23705,#23706,#23707),.UNSPECIFIED.,.F.,.F.,(4,1,1,1,1,1,
1,4),(47.123889803847,48.0779977182254,49.0725690682629,50.0671404183004,
51.061711768338,52.0562831183755,53.050854468413,53.4070751110266),
 .UNSPECIFIED.);
#241=B_SPLINE_CURVE_WITH_KNOTS('',3,(#23712,#23713,#23714,#23715,#23716,
#23717,#23718,#23719,#23720,#23721),.UNSPECIFIED.,.F.,.F.,(4,1,1,1,1,1,
1,4),(40.8407044966674,41.4521128889653,42.4466842390029,43.4412555890404,
44.4358269390779,45.4303982891154,46.424969639153,47.123889803847),
 .UNSPECIFIED.);
#242=B_SPLINE_CURVE_WITH_KNOTS('',3,(#23722,#23723,#23724,#23725,#23726,
#23727,#23728,#23729,#23730,#23731,#23732),.UNSPECIFIED.,.F.,.F.,(4,1,1,
1,1,1,1,1,4),(40.8407044966674,41.1159982679627,42.1105696180002,43.1051409680378,
44.0997123180753,45.0942836681128,46.0888550181503,47.0834263681879,47.123889803847),
 .UNSPECIFIED.);
#243=B_SPLINE_CURVE_WITH_KNOTS('',3,(#23737,#23738,#23739,#23740,#23741,
#23742,#23743,#23744,#23745,#23746),.UNSPECIFIED.,.F.,.F.,(4,1,1,1,1,1,
1,4),(34.5575191894878,35.4846847887402,36.4792561387777,37.4738274888152,
38.4683988388528,39.4629701888903,40.4575415389278,40.8407044966674),
 .UNSPECIFIED.);
#244=B_SPLINE_CURVE_WITH_KNOTS('',3,(#23747,#23748,#23749,#23750,#23751,
#23752,#23753,#23754,#23755,#23756),.UNSPECIFIED.,.F.,.F.,(4,1,1,1,1,1,
1,4),(34.5575191894878,35.1485701677375,36.1431415177751,37.1377128678126,
38.1322842178501,39.1268555678876,40.1214269179252,40.8407044966674),
 .UNSPECIFIED.);
#245=B_SPLINE_CURVE_WITH_KNOTS('',3,(#23761,#23762,#23763,#23764,#23765,
#23766,#23767,#23768,#23769,#23770,#23771),.UNSPECIFIED.,.F.,.F.,(4,1,1,
1,1,1,1,1,4),(28.2743338823082,28.5226853384775,29.517256688515,30.5118280385526,
31.5063993885901,32.5009707386276,33.4955420886651,34.4901134387027,34.5575191894878),
 .UNSPECIFIED.);
#246=B_SPLINE_CURVE_WITH_KNOTS('',3,(#23772,#23773,#23774,#23775,#23776,
#23777,#23778,#23779,#23780,#23781),.UNSPECIFIED.,.F.,.F.,(4,1,1,1,1,1,
1,4),(28.2743338823082,29.1811420675124,30.1757134175499,31.1702847675875,
32.164856117625,33.1594274676625,34.1539988177,34.5575191894878),
 .UNSPECIFIED.);
#247=B_SPLINE_CURVE_WITH_KNOTS('',3,(#23786,#23787,#23788,#23789,#23790,
#23791,#23792,#23793,#23794,#23795),.UNSPECIFIED.,.F.,.F.,(4,1,1,1,1,1,
1,4),(21.9911485751286,22.5552572382524,23.5498285882899,24.5443999383274,
25.5389712883649,26.5335426384025,27.52811398844,28.2743338823082),
 .UNSPECIFIED.);
#248=B_SPLINE_CURVE_WITH_KNOTS('',3,(#23796,#23797,#23798,#23799,#23800,
#23801,#23802,#23803,#23804,#23805,#23806),.UNSPECIFIED.,.F.,.F.,(4,1,1,
1,1,1,1,1,4),(21.9911485751286,22.2191426172497,23.2137139672872,24.2082853173248,
25.2028566673623,26.1974280173998,27.1919993674374,28.1865707174749,28.2743338823082),
 .UNSPECIFIED.);
#249=B_SPLINE_CURVE_WITH_KNOTS('',3,(#23811,#23812,#23813,#23814,#23815,
#23816,#23817,#23818,#23819,#23820),.UNSPECIFIED.,.F.,.F.,(4,1,1,1,1,1,
1,4),(15.707963267949,16.5878291380272,17.5824004880647,18.5769718381023,
19.5715431881398,20.5661145381773,21.5606858882148,21.9911485751286),
 .UNSPECIFIED.);
#250=B_SPLINE_CURVE_WITH_KNOTS('',3,(#23821,#23822,#23823,#23824,#23825,
#23826,#23827,#23828,#23829,#23830),.UNSPECIFIED.,.F.,.F.,(4,1,1,1,1,1,
1,4),(15.707963267949,16.2517145170246,17.2462858670621,18.2408572170996,
19.2354285671371,20.2299999171747,21.2245712672122,21.9911485751286),
 .UNSPECIFIED.);
#251=B_SPLINE_CURVE_WITH_KNOTS('',3,(#24063,#24064,#24065,#24066,#24067,
#24068,#24069,#24070,#24071,#24072,#24073,#24074,#24075,#24076,#24077,#24078,
#24079,#24080,#24081,#24082,#24083,#24084,#24085,#24086,#24087,#24088,#24089,
#24090,#24091,#24092,#24093,#24094,#24095,#24096,#24097,#24098,#24099,#24100,
#24101,#24102,#24103,#24104,#24105,#24106,#24107,#24108,#24109,#24110,#24111,
#24112,#24113,#24114,#24115,#24116,#24117,#24118,#24119,#24120,#24121,#24122,
#24123,#24124,#24125,#24126,#24127,#24128,#24129,#24130,#24131,#24132,#24133,
#24134,#24135,#24136,#24137,#24138,#24139,#24140,#24141,#24142,#24143,#24144,
#24145,#24146,#24147,#24148,#24149,#24150,#24151,#24152,#24153,#24154,#24155,
#24156,#24157,#24158,#24159),.UNSPECIFIED.,.F.,.F.,(4,3,3,3,3,3,3,3,3,3,
3,3,3,3,3,3,3,3,3,3,3,3,3,3,3,3,3,3,3,3,3,3,4),(-0.780432929098692,-0.744171076506414,
-0.707269362542449,-0.685703619005375,-0.677641063801082,-0.671987810898122,
-0.635377863422115,-0.601232813738007,-0.58629435450121,-0.577918583648485,
-0.570482007246046,-0.534001224941446,-0.497606122019792,-0.462171004484833,
-0.437182619850938,-0.428169806816731,-0.422783055253062,-0.387505838307544,
-0.362217465949252,-0.326639251159082,-0.290748131513672,-0.281156185824485,
-0.276193604589621,-0.241028956991022,-0.205655214290034,-0.170550703428344,
-0.149231865499801,-0.141809112984284,-0.135579482248505,-0.100965757631287,
-0.0667517818268251,-0.0333758909134126,0.),.UNSPECIFIED.);
#252=B_SPLINE_CURVE_WITH_KNOTS('',3,(#24160,#24161,#24162,#24163,#24164,
#24165,#24166,#24167,#24168,#24169,#24170,#24171,#24172,#24173,#24174,#24175,
#24176,#24177,#24178,#24179,#24180,#24181,#24182,#24183,#24184,#24185,#24186,
#24187,#24188,#24189,#24190,#24191,#24192,#24193,#24194,#24195,#24196,#24197,
#24198,#24199,#24200,#24201,#24202,#24203,#24204,#24205,#24206,#24207,#24208,
#24209,#24210,#24211,#24212,#24213,#24214,#24215,#24216,#24217,#24218,#24219,
#24220,#24221,#24222,#24223,#24224,#24225,#24226,#24227,#24228,#24229,#24230,
#24231,#24232,#24233,#24234,#24235,#24236,#24237,#24238,#24239,#24240,#24241,
#24242,#24243,#24244,#24245,#24246,#24247,#24248,#24249,#24250,#24251,#24252,
#24253,#24254,#24255,#24256),.UNSPECIFIED.,.F.,.F.,(4,3,3,3,3,3,3,3,3,3,
3,3,3,3,3,3,3,3,3,3,3,3,3,3,3,3,3,3,3,3,3,3,4),(-0.782320427274638,-0.749691875557366,
-0.716079002773824,-0.69538894405227,-0.688774800459675,-0.682477718221598,
-0.648343944567492,-0.615430709400175,-0.601031169014474,-0.592885555855582,
-0.587118698134123,-0.551838327246284,-0.516166914508928,-0.48087202150747,
-0.456913531937842,-0.450542037325468,-0.445610077462954,-0.409473029571469,
-0.385038063228958,-0.349835104468143,-0.31400993863385,-0.305067953562657,
-0.298844713484155,-0.261489124298636,-0.224910226260933,-0.188134349953557,
-0.164617556209363,-0.155035509146063,-0.149135266247745,-0.111810553481794,
-0.0745528270350788,-0.0372764135175394,0.),.UNSPECIFIED.);
#253=B_SPLINE_CURVE_WITH_KNOTS('',3,(#24973,#24974,#24975,#24976,#24977,
#24978,#24979,#24980,#24981,#24982),.UNSPECIFIED.,.F.,.F.,(4,3,3,4),(170.775637537894,
171.066272206454,172.060843556492,172.96352513604),.UNSPECIFIED.);
#254=B_SPLINE_CURVE_WITH_KNOTS('',3,(#24984,#24985,#24986,#24987,#24988,
#24989,#24990,#24991,#24992,#24993,#24994,#24995,#24996,#24997,#24998,#24999,
#25000,#25001,#25002,#25003,#25004,#25005,#25006,#25007,#25008,#25009,#25010,
#25011,#25012,#25013,#25014,#25015,#25016,#25017,#25018,#25019,#25020,#25021,
#25022,#25023,#25024,#25025,#25026,#25027,#25028,#25029,#25030,#25031,#25032,
#25033,#25034,#25035,#25036,#25037,#25038,#25039,#25040,#25041,#25042,#25043,
#25044,#25045,#25046,#25047,#25048,#25049,#25050,#25051,#25052,#25053,#25054,
#25055,#25056,#25057,#25058,#25059,#25060,#25061,#25062,#25063,#25064,#25065,
#25066,#25067,#25068,#25069,#25070,#25071,#25072,#25073,#25074,#25075,#25076,
#25077,#25078,#25079,#25080),.UNSPECIFIED.,.F.,.F.,(4,3,3,3,3,3,3,3,3,3,
3,3,3,3,3,3,3,3,3,3,3,3,3,3,3,3,3,3,3,3,3,3,4),(-0.782320427274655,-0.749691875557393,
-0.716078998607798,-0.695388940146623,-0.688774779534789,-0.68247771551652,
-0.648343938050999,-0.615430703698248,-0.601031163668919,-0.592885529328257,
-0.587118690997954,-0.551838318465963,-0.516166905662748,-0.48087201177489,
-0.456913524638415,-0.450542066424711,-0.445610092428472,-0.409473044351031,
-0.385038063228989,-0.349835101082961,-0.314009932195594,-0.305067936627418,
-0.298844709169275,-0.261489120523116,-0.224910219813707,-0.188134343389742,
-0.164617550466024,-0.155035492002945,-0.149135262336089,-0.111810548816022,
-0.074552824760043,-0.0372764123800215,0.),.UNSPECIFIED.);
#255=B_SPLINE_CURVE_WITH_KNOTS('',3,(#25081,#25082,#25083,#25084,#25085,
#25086,#25087,#25088,#25089),.UNSPECIFIED.,.F.,.F.,(4,1,1,1,1,1,4),(10.3761761872891,
11.2788577668369,12.2734291168745,13.268000466912,14.2625718169495,15.257143166987,
15.707963267949),.UNSPECIFIED.);
#256=B_SPLINE_CURVE_WITH_KNOTS('',3,(#25095,#25096,#25097,#25098,#25099,
#25100,#25101,#25102,#25103,#25104,#25105,#25106,#25107,#25108,#25109,#25110,
#25111,#25112,#25113,#25114,#25115,#25116,#25117,#25118,#25119,#25120,#25121,
#25122,#25123,#25124,#25125,#25126,#25127,#25128,#25129,#25130,#25131,#25132,
#25133,#25134,#25135,#25136,#25137,#25138,#25139,#25140,#25141,#25142,#25143,
#25144,#25145,#25146,#25147,#25148,#25149,#25150,#25151,#25152,#25153,#25154,
#25155,#25156,#25157,#25158,#25159,#25160,#25161,#25162,#25163,#25164,#25165,
#25166,#25167,#25168,#25169,#25170,#25171,#25172,#25173,#25174,#25175,#25176,
#25177,#25178,#25179,#25180,#25181,#25182,#25183,#25184,#25185,#25186,#25187,
#25188,#25189,#25190,#25191),.UNSPECIFIED.,.F.,.F.,(4,3,3,3,3,3,3,3,3,3,
3,3,3,3,3,3,3,3,3,3,3,3,3,3,3,3,3,3,3,3,3,3,4),(-0.780432929098614,-0.744171076506339,
-0.70726936348061,-0.685703619884899,-0.677641067625544,-0.671987820717708,
-0.635377874072834,-0.601232823057384,-0.586294363238125,-0.577918591325873,
-0.570482007745035,-0.534001225423256,-0.497606123558654,-0.462171010723763,
-0.437182624530132,-0.428169820114518,-0.422783054578572,-0.387505840929447,
-0.362217465949239,-0.326639254971974,-0.290748136090389,-0.281156242639861,
-0.27619361681087,-0.241028972315843,-0.205655229311345,-0.170550714021067,
-0.149231874768433,-0.141809159915445,-0.135579488063576,-0.100965760056957,
-0.0667517778475045,-0.0333758889237523,0.),.UNSPECIFIED.);
#257=B_SPLINE_CURVE_WITH_KNOTS('',3,(#25194,#25195,#25196,#25197,#25198,
#25199,#25200,#25201),.UNSPECIFIED.,.F.,.F.,(4,1,1,1,1,4),(11.6149723878396,
12.6095437378771,13.6041150879146,14.5986864379522,15.5932577879897,15.707963267949),
 .UNSPECIFIED.);
#258=B_SPLINE_CURVE_WITH_KNOTS('',3,(#25918,#25919,#25920,#25921,#25922,
#25923,#25924),.UNSPECIFIED.,.F.,.F.,(4,3,4),(-175.044557606604,-174.049986256567,
-173.738994173958),.UNSPECIFIED.);
#259=B_SPLINE_CURVE_WITH_KNOTS('',3,(#26240,#26241,#26242,#26243),
 .UNSPECIFIED.,.F.,.F.,(4,4),(0.0531689808046697,0.0554215660138355),
 .UNSPECIFIED.);
#260=B_SPLINE_CURVE_WITH_KNOTS('',3,(#26251,#26252,#26253,#26254),
 .UNSPECIFIED.,.F.,.F.,(4,4),(0.,0.00224311679852086),.UNSPECIFIED.);
#261=B_SPLINE_CURVE_WITH_KNOTS('',3,(#26379,#26380,#26381,#26382,#26383,
#26384),.UNSPECIFIED.,.F.,.F.,(4,2,4),(0.120171671798206,0.144386237549695,
0.158573008898185),.UNSPECIFIED.);
#262=B_SPLINE_CURVE_WITH_KNOTS('',3,(#26393,#26394,#26395,#26396,#26397,
#26398,#26399,#26400,#26401,#26402),.UNSPECIFIED.,.F.,.F.,(4,2,2,2,4),(0.0817703346982273,
0.0959571060467179,0.120171671798206,0.144386237549695,0.158573008898185),
 .UNSPECIFIED.);
#263=B_SPLINE_CURVE_WITH_KNOTS('',3,(#26411,#26412,#26413,#26414,#26415,
#26416,#26417,#26418,#26419,#26420),.UNSPECIFIED.,.F.,.F.,(4,2,2,2,4),(0.0817703346982278,
0.095957106046718,0.120171671798206,0.144386237549695,0.158573008898185),
 .UNSPECIFIED.);
#264=B_SPLINE_CURVE_WITH_KNOTS('',3,(#26429,#26430,#26431,#26432,#26433,
#26434,#26435,#26436,#26437,#26438),.UNSPECIFIED.,.F.,.F.,(4,2,2,2,4),(0.0817703346982272,
0.0959571060467179,0.120171671798206,0.144386237549695,0.158573008898185),
 .UNSPECIFIED.);
#265=B_SPLINE_CURVE_WITH_KNOTS('',3,(#26447,#26448,#26449,#26450,#26451,
#26452,#26453,#26454,#26455,#26456),.UNSPECIFIED.,.F.,.F.,(4,2,2,2,4),(0.0817703346982273,
0.0959571060467178,0.120171671798206,0.144386237549695,0.158573008898185),
 .UNSPECIFIED.);
#266=B_SPLINE_CURVE_WITH_KNOTS('',3,(#26465,#26466,#26467,#26468,#26469,
#26470,#26471,#26472,#26473,#26474),.UNSPECIFIED.,.F.,.F.,(4,2,2,2,4),(0.081770334698227,
0.0959571060467179,0.120171671798206,0.144386237549695,0.158573008898185),
 .UNSPECIFIED.);
#267=B_SPLINE_CURVE_WITH_KNOTS('',3,(#26483,#26484,#26485,#26486,#26487,
#26488,#26489,#26490,#26491,#26492),.UNSPECIFIED.,.F.,.F.,(4,2,2,2,4),(0.0817703346982273,
0.0959571060467179,0.120171671798206,0.144386237549695,0.158573008898185),
 .UNSPECIFIED.);
#268=B_SPLINE_CURVE_WITH_KNOTS('',3,(#26496,#26497,#26498,#26499,#26500,
#26501,#26502,#26503,#26504),.UNSPECIFIED.,.F.,.F.,(4,1,1,1,1,1,4),(-0.20552137705515,
-0.181579319698556,-0.13245320137828,-0.107890142218142,-0.0833270830580044,
-0.0587640238978664,-0.0348207934698036),.UNSPECIFIED.);
#269=B_SPLINE_CURVE_WITH_KNOTS('',3,(#26506,#26507,#26508,#26509,#26510,
#26511,#26512,#26513,#26514,#26515),.UNSPECIFIED.,.F.,.F.,(4,2,2,2,4),(0.0817703346982273,
0.0959571060467179,0.120171671798206,0.144386237549695,0.158573008898185),
 .UNSPECIFIED.);
#270=B_SPLINE_CURVE_WITH_KNOTS('',3,(#26524,#26525,#26526,#26527,#26528,
#26529,#26530,#26531,#26532,#26533),.UNSPECIFIED.,.F.,.F.,(4,2,2,2,4),(0.0817703346982272,
0.095957106046718,0.120171671798206,0.144386237549695,0.158573008898185),
 .UNSPECIFIED.);
#271=B_SPLINE_CURVE_WITH_KNOTS('',3,(#26542,#26543,#26544,#26545,#26546,
#26547,#26548,#26549,#26550,#26551),.UNSPECIFIED.,.F.,.F.,(4,2,2,2,4),(0.0817703346982275,
0.095957106046718,0.120171671798206,0.144386237549695,0.158573008898185),
 .UNSPECIFIED.);
#272=B_SPLINE_CURVE_WITH_KNOTS('',3,(#26560,#26561,#26562,#26563,#26564,
#26565,#26566,#26567,#26568,#26569),.UNSPECIFIED.,.F.,.F.,(4,2,2,2,4),(0.0817703346982276,
0.095957106046718,0.120171671798206,0.144386237549695,0.158573008898185),
 .UNSPECIFIED.);
#273=B_SPLINE_CURVE_WITH_KNOTS('',3,(#26578,#26579,#26580,#26581,#26582,
#26583,#26584,#26585,#26586,#26587),.UNSPECIFIED.,.F.,.F.,(4,2,2,2,4),(0.0817703346982272,
0.0959571060467178,0.120171671798206,0.144386237549695,0.158573008898185),
 .UNSPECIFIED.);
#274=B_SPLINE_CURVE_WITH_KNOTS('',3,(#26596,#26597,#26598,#26599,#26600,
#26601,#26602,#26603,#26604,#26605),.UNSPECIFIED.,.F.,.F.,(4,2,2,2,4),(0.0817703346982273,
0.0959571060467179,0.120171671798206,0.144386237549695,0.158573008898185),
 .UNSPECIFIED.);
#275=B_SPLINE_CURVE_WITH_KNOTS('',3,(#26614,#26615,#26616,#26617,#26618,
#26619,#26620,#26621,#26622,#26623),.UNSPECIFIED.,.F.,.F.,(4,2,2,2,4),(0.0817703346982272,
0.0959571060467179,0.120171671798206,0.144386237549695,0.158573008898185),
 .UNSPECIFIED.);
#276=B_SPLINE_CURVE_WITH_KNOTS('',3,(#26632,#26633,#26634,#26635,#26636,
#26637,#26638,#26639,#26640,#26641),.UNSPECIFIED.,.F.,.F.,(4,2,2,2,4),(0.0817703346982276,
0.095957106046718,0.120171671798206,0.144386237549695,0.158573008898185),
 .UNSPECIFIED.);
#277=B_SPLINE_CURVE_WITH_KNOTS('',3,(#26649,#26650,#26651,#26652,#26653,
#26654),.UNSPECIFIED.,.F.,.F.,(4,2,4),(0.0817703346982272,0.0959571060467178,
0.120171671798206),.UNSPECIFIED.);
#278=B_SPLINE_CURVE_WITH_KNOTS('',3,(#26809,#26810,#26811,#26812,#26813,
#26814,#26815,#26816,#26817),.UNSPECIFIED.,.F.,.F.,(4,1,1,1,1,1,4),(0.0581066990795184,
0.0587640238978664,0.0833270830580044,0.107890142218142,0.13245320137828,
0.181579319698556,0.182236644516894),.UNSPECIFIED.);
#279=B_SPLINE_CURVE_WITH_KNOTS('',3,(#26818,#26819,#26820,#26821,#26822,
#26823,#26824,#26825),.UNSPECIFIED.,.F.,.F.,(4,2,2,4),(0.,0.0126311894885661,
0.032486538769803,0.052794817339328),.UNSPECIFIED.);
#280=B_SPLINE_CURVE_WITH_KNOTS('',3,(#26826,#26827,#26828,#26829,#26830,
#26831,#26832,#26833,#26834,#26835,#26836,#26837,#26838,#26839,#26840,#26841,
#26842,#26843,#26844,#26845,#26846,#26847,#26848,#26849,#26850),
 .UNSPECIFIED.,.F.,.F.,(4,3,3,3,3,3,3,3,4),(0.,0.011920157067792,0.0235023431475078,
0.0268086068446529,0.0354226971140202,0.0406217026705462,0.0495092313150064,
0.0577137413084294,0.0614436123664036),.UNSPECIFIED.);
#281=B_SPLINE_CURVE_WITH_KNOTS('',3,(#26983,#26984,#26985,#26986,#26987,
#26988,#26989,#26990,#26991,#26992),.UNSPECIFIED.,.F.,.F.,(4,3,3,4),(-4.09254174883829,
-3.98610650986719,-2.98957988240039,-2.06514013327809),.UNSPECIFIED.);
#282=B_SPLINE_CURVE_WITH_KNOTS('',3,(#26995,#26996,#26997,#26998,#26999,
#27000,#27001),.UNSPECIFIED.,.F.,.F.,(4,3,4),(0.,0.996526627466801,1.11419103802947),
 .UNSPECIFIED.);
#283=B_SPLINE_CURVE_WITH_KNOTS('',3,(#27006,#27007,#27008,#27009,#27010,
#27011,#27012,#27013,#27014,#27015,#27016,#27017,#27018,#27019,#27020,#27021,
#27022,#27023,#27024,#27025,#27026,#27027),.UNSPECIFIED.,.F.,.F.,(4,3,3,
3,3,3,3,4),(-10.3757270560179,-9.96526627466798,-8.96873964720119,-7.97221301973439,
-6.97568639226759,-5.97915976480079,-4.98263313733399,-4.09254174883829),
 .UNSPECIFIED.);
#284=B_SPLINE_CURVE_WITH_KNOTS('',3,(#27028,#27029,#27030,#27031,#27032,
#27033,#27034,#27035,#27036,#27037,#27038,#27039,#27040,#27041,#27042,#27043,
#27044,#27045,#27046,#27047,#27048,#27049),.UNSPECIFIED.,.F.,.F.,(4,3,3,
3,3,3,3,4),(1.11419103802947,1.9930532549336,2.9895798824004,3.98610650986719,
4.98263313733399,5.97915976480079,6.97568639226759,7.39737634520906),
 .UNSPECIFIED.);
#285=B_SPLINE_CURVE_WITH_KNOTS('',3,(#27054,#27055,#27056,#27057,#27058,
#27059,#27060,#27061,#27062,#27063,#27064,#27065,#27066,#27067,#27068,#27069,
#27070,#27071,#27072,#27073,#27074,#27075),.UNSPECIFIED.,.F.,.F.,(4,3,3,
3,3,3,3,4),(-16.6589123631975,-15.9444260394688,-14.947899412002,-13.9513727845352,
-12.9548461570684,-11.9583195296016,-10.9617929021348,-10.3757270560179),
 .UNSPECIFIED.);
#286=B_SPLINE_CURVE_WITH_KNOTS('',3,(#27076,#27077,#27078,#27079,#27080,
#27081,#27082,#27083,#27084,#27085,#27086,#27087,#27088,#27089,#27090,#27091,
#27092,#27093,#27094,#27095,#27096,#27097),.UNSPECIFIED.,.F.,.F.,(4,3,3,
3,3,3,3,4),(7.39737634520906,7.97221301973439,8.96873964720119,9.96526627466799,
10.9617929021348,11.9583195296016,12.9548461570684,13.6805616523886),
 .UNSPECIFIED.);
#287=B_SPLINE_CURVE_WITH_KNOTS('',3,(#27102,#27103,#27104,#27105,#27106,
#27107,#27108,#27109,#27110,#27111,#27112,#27113,#27114,#27115,#27116,#27117,
#27118,#27119,#27120,#27121,#27122,#27123,#27124,#27125,#27126),
 .UNSPECIFIED.,.F.,.F.,(4,3,3,3,3,3,3,3,4),(-22.942097670377,-22.9201124317364,
-21.9235858042696,-20.9270591768028,-19.930532549336,-18.9340059218692,
-17.9374792944024,-16.9409526669356,-16.6589123631975),.UNSPECIFIED.);
#288=B_SPLINE_CURVE_WITH_KNOTS('',3,(#27127,#27128,#27129,#27130,#27131,
#27132,#27133,#27134,#27135,#27136,#27137,#27138,#27139,#27140,#27141,#27142,
#27143,#27144,#27145,#27146,#27147,#27148,#27149,#27150,#27151),
 .UNSPECIFIED.,.F.,.F.,(4,3,3,3,3,3,3,3,4),(13.6805616523886,13.9513727845352,
14.947899412002,15.9444260394688,16.9409526669356,17.9374792944024,18.9340059218692,
19.930532549336,19.9637469595682),.UNSPECIFIED.);
#289=B_SPLINE_CURVE_WITH_KNOTS('',3,(#27156,#27157,#27158,#27159,#27160,
#27161,#27162,#27163,#27164,#27165,#27166,#27167,#27168,#27169,#27170,#27171,
#27172,#27173,#27174,#27175,#27176,#27177),.UNSPECIFIED.,.F.,.F.,(4,3,3,
3,3,3,3,4),(-29.2252829775566,-28.8992721965371,-27.9027455690703,-26.9062189416035,
-25.9096923141368,-24.91316568667,-23.9166390592032,-22.942097670377),
 .UNSPECIFIED.);
#290=B_SPLINE_CURVE_WITH_KNOTS('',3,(#27178,#27179,#27180,#27181,#27182,
#27183,#27184,#27185,#27186,#27187,#27188,#27189,#27190,#27191,#27192,#27193,
#27194,#27195,#27196,#27197,#27198,#27199),.UNSPECIFIED.,.F.,.F.,(4,3,3,
3,3,3,3,4),(19.9637469595682,20.9270591768028,21.9235858042696,22.9201124317364,
23.9166390592031,24.91316568667,25.9096923141368,26.2469322667478),
 .UNSPECIFIED.);
#291=B_SPLINE_CURVE_WITH_KNOTS('',3,(#27204,#27205,#27206,#27207,#27208,
#27209,#27210,#27211,#27212,#27213,#27214,#27215,#27216,#27217,#27218,#27219,
#27220,#27221,#27222,#27223,#27224,#27225),.UNSPECIFIED.,.F.,.F.,(4,3,3,
3,3,3,3,4),(-35.5084682847362,-34.8784319613379,-33.8819053338711,-32.8853787064043,
-31.8888520789375,-30.8923254514707,-29.8957988240039,-29.2252829775566),
 .UNSPECIFIED.);
#292=B_SPLINE_CURVE_WITH_KNOTS('',3,(#27226,#27227,#27228,#27229,#27230,
#27231,#27232,#27233,#27234,#27235,#27236,#27237,#27238,#27239,#27240,#27241,
#27242,#27243,#27244,#27245,#27246,#27247),.UNSPECIFIED.,.F.,.F.,(4,3,3,
3,3,3,3,4),(26.2469322667478,26.9062189416035,27.9027455690703,28.8992721965371,
29.895798824004,30.8923254514707,31.8888520789375,32.5301175739274),
 .UNSPECIFIED.);
#293=B_SPLINE_CURVE_WITH_KNOTS('',3,(#27252,#27253,#27254,#27255,#27256,
#27257,#27258,#27259,#27260,#27261,#27262,#27263,#27264,#27265,#27266,#27267,
#27268,#27269,#27270,#27271,#27272,#27273),.UNSPECIFIED.,.F.,.F.,(4,3,3,
3,3,3,3,4),(-41.7916535919158,-40.8575917261387,-39.8610650986719,-38.8645384712051,
-37.8680118437383,-36.8714852162715,-35.8749585888047,-35.5084682847362),
 .UNSPECIFIED.);
#294=B_SPLINE_CURVE_WITH_KNOTS('',3,(#27274,#27275,#27276,#27277,#27278,
#27279,#27280,#27281,#27282,#27283,#27284,#27285,#27286,#27287,#27288,#27289,
#27290,#27291,#27292,#27293,#27294,#27295),.UNSPECIFIED.,.F.,.F.,(4,3,3,
3,3,3,3,4),(32.5301175739274,32.8853787064043,33.8819053338711,34.8784319613379,
35.8749585888047,36.8714852162715,37.8680118437383,38.813302881107),
 .UNSPECIFIED.);
#295=B_SPLINE_CURVE_WITH_KNOTS('',3,(#27300,#27301,#27302,#27303,#27304,
#27305,#27306,#27307,#27308,#27309,#27310,#27311,#27312,#27313,#27314,#27315,
#27316,#27317,#27318,#27319,#27320,#27321,#27322,#27323,#27324),
 .UNSPECIFIED.,.F.,.F.,(4,3,3,3,3,3,3,3,4),(-48.0748388990954,-47.8332781184063,
-46.8367514909395,-45.8402248634727,-44.8436982360059,-43.8471716085391,
-42.8506449810723,-41.8541183536055,-41.7916535919158),.UNSPECIFIED.);
#296=B_SPLINE_CURVE_WITH_KNOTS('',3,(#27325,#27326,#27327,#27328,#27329,
#27330,#27331,#27332,#27333,#27334,#27335,#27336,#27337,#27338,#27339,#27340,
#27341,#27342,#27343,#27344,#27345,#27346,#27347,#27348,#27349),
 .UNSPECIFIED.,.F.,.F.,(4,3,3,3,3,3,3,3,4),(38.813302881107,38.8645384712051,
39.8610650986719,40.8575917261387,41.8541183536055,42.8506449810723,43.8471716085391,
44.8436982360059,45.0964881882866),.UNSPECIFIED.);
#297=B_SPLINE_CURVE_WITH_KNOTS('',3,(#27354,#27355,#27356,#27357,#27358,
#27359,#27360,#27361,#27362,#27363,#27364,#27365,#27366,#27367,#27368,#27369,
#27370,#27371,#27372,#27373,#27374,#27375),.UNSPECIFIED.,.F.,.F.,(4,3,3,
3,3,3,3,4),(-54.358024206275,-53.8124378832071,-52.8159112557403,-51.8193846282735,
-50.8228580008067,-49.8263313733399,-48.8298047458731,-48.0748388990954),
 .UNSPECIFIED.);
#298=B_SPLINE_CURVE_WITH_KNOTS('',3,(#27376,#27377,#27378,#27379,#27380,
#27381,#27382,#27383,#27384,#27385,#27386,#27387,#27388,#27389,#27390,#27391,
#27392,#27393,#27394,#27395,#27396,#27397),.UNSPECIFIED.,.F.,.F.,(4,3,3,
3,3,3,3,4),(45.0964881882866,45.8402248634727,46.8367514909395,47.8332781184063,
48.8298047458731,49.8263313733399,50.8228580008067,51.3796734954662),
 .UNSPECIFIED.);
#299=B_SPLINE_CURVE_WITH_KNOTS('',3,(#27402,#27403,#27404,#27405,#27406,
#27407,#27408,#27409,#27410,#27411,#27412,#27413,#27414,#27415,#27416,#27417,
#27418,#27419,#27420,#27421,#27422,#27423),.UNSPECIFIED.,.F.,.F.,(4,3,3,
3,3,3,3,4),(-60.6412095134546,-59.7915976480079,-58.7950710205411,-57.7985443930743,
-56.8020177656075,-55.8054911381407,-54.8089645106739,-54.358024206275),
 .UNSPECIFIED.);
#300=B_SPLINE_CURVE_WITH_KNOTS('',3,(#27424,#27425,#27426,#27427,#27428,
#27429,#27430,#27431,#27432,#27433,#27434,#27435,#27436,#27437,#27438,#27439,
#27440,#27441,#27442,#27443,#27444,#27445),.UNSPECIFIED.,.F.,.F.,(4,3,3,
3,3,3,3,4),(51.3796734954662,51.8193846282735,52.8159112557403,53.8124378832071,
54.8089645106739,55.8054911381407,56.8020177656075,57.6628588026458),
 .UNSPECIFIED.);
#301=B_SPLINE_CURVE_WITH_KNOTS('',3,(#27450,#27451,#27452,#27453,#27454,
#27455,#27456,#27457,#27458,#27459,#27460,#27461,#27462,#27463,#27464,#27465,
#27466,#27467,#27468,#27469,#27470,#27471,#27472,#27473,#27474),
 .UNSPECIFIED.,.F.,.F.,(4,3,3,3,3,3,3,3,4),(-66.9243948206342,-66.7672840402755,
-65.7707574128087,-64.7742307853419,-63.7777041578751,-62.7811775304083,
-61.7846509029415,-60.7881242754747,-60.6412095134546),.UNSPECIFIED.);
#302=B_SPLINE_CURVE_WITH_KNOTS('',3,(#27475,#27476,#27477,#27478,#27479,
#27480,#27481,#27482,#27483,#27484,#27485,#27486,#27487,#27488,#27489,#27490,
#27491,#27492,#27493,#27494,#27495,#27496,#27497,#27498,#27499),
 .UNSPECIFIED.,.F.,.F.,(4,3,3,3,3,3,3,3,4),(57.6628588026458,57.7985443930743,
58.7950710205411,59.7915976480079,60.7881242754747,61.7846509029415,62.7811775304083,
63.7777041578751,63.9460441098254),.UNSPECIFIED.);
#303=B_SPLINE_CURVE_WITH_KNOTS('',3,(#27504,#27505,#27506,#27507,#27508,
#27509,#27510,#27511,#27512,#27513,#27514,#27515,#27516,#27517,#27518,#27519,
#27520,#27521,#27522,#27523,#27524,#27525),.UNSPECIFIED.,.F.,.F.,(4,3,3,
3,3,3,3,4),(-73.2075801278138,-72.7464438050762,-71.7499171776095,-70.7533905501426,
-69.7568639226759,-68.760337295209,-67.7638106677423,-66.9243948206342),
 .UNSPECIFIED.);
#304=B_SPLINE_CURVE_WITH_KNOTS('',3,(#27526,#27527,#27528,#27529,#27530,
#27531,#27532,#27533,#27534,#27535,#27536,#27537,#27538,#27539,#27540,#27541,
#27542,#27543,#27544,#27545,#27546,#27547),.UNSPECIFIED.,.F.,.F.,(4,3,3,
3,3,3,3,4),(63.9460441098254,64.7742307853419,65.7707574128087,66.7672840402755,
67.7638106677423,68.7603372952091,69.7568639226759,70.229229417005),
 .UNSPECIFIED.);
#305=B_SPLINE_CURVE_WITH_KNOTS('',3,(#27552,#27553,#27554,#27555,#27556,
#27557,#27558,#27559,#27560,#27561,#27562,#27563,#27564,#27565,#27566,#27567,
#27568,#27569,#27570,#27571,#27572,#27573),.UNSPECIFIED.,.F.,.F.,(4,3,3,
3,3,3,3,4),(-79.4907654349934,-78.725603569877,-77.7290769424102,-76.7325503149434,
-75.7360236874766,-74.7394970600099,-73.742970432543,-73.2075801278138),
 .UNSPECIFIED.);
#306=B_SPLINE_CURVE_WITH_KNOTS('',3,(#27574,#27575,#27576,#27577,#27578,
#27579,#27580,#27581,#27582,#27583,#27584,#27585,#27586,#27587,#27588,#27589,
#27590,#27591,#27592,#27593,#27594,#27595),.UNSPECIFIED.,.F.,.F.,(4,3,3,
3,3,3,3,4),(70.229229417005,70.7533905501427,71.7499171776095,72.7464438050763,
73.7429704325431,74.7394970600099,75.7360236874767,76.5124147241846),
 .UNSPECIFIED.);
#307=B_SPLINE_CURVE_WITH_KNOTS('',3,(#27600,#27601,#27602,#27603,#27604,
#27605,#27606,#27607,#27608,#27609,#27610,#27611,#27612,#27613,#27614,#27615,
#27616,#27617,#27618,#27619,#27620,#27621,#27622,#27623,#27624),
 .UNSPECIFIED.,.F.,.F.,(4,3,3,3,3,3,3,3,4),(-85.773950742173,-85.7012899621446,
-84.7047633346778,-83.708236707211,-82.7117100797442,-81.7151834522774,
-80.7186568248106,-79.7221301973438,-79.4907654349934),.UNSPECIFIED.);
#308=B_SPLINE_CURVE_WITH_KNOTS('',3,(#27625,#27626,#27627,#27628,#27629,
#27630,#27631,#27632,#27633,#27634,#27635,#27636,#27637,#27638,#27639,#27640,
#27641,#27642,#27643,#27644,#27645,#27646,#27647,#27648,#27649),
 .UNSPECIFIED.,.F.,.F.,(4,3,3,3,3,3,3,3,4),(76.5124147241846,76.7325503149435,
77.7290769424103,78.7256035698771,79.7221301973439,80.7186568248107,81.7151834522775,
82.7117100797443,82.7956000313641),.UNSPECIFIED.);
#309=B_SPLINE_CURVE_WITH_KNOTS('',3,(#27654,#27655,#27656,#27657,#27658,
#27659,#27660,#27661,#27662,#27663,#27664,#27665,#27666,#27667,#27668,#27669,
#27670,#27671,#27672,#27673,#27674,#27675),.UNSPECIFIED.,.F.,.F.,(4,3,3,
3,3,3,3,4),(-92.0571360493526,-91.6804497269454,-90.6839230994786,-89.6873964720118,
-88.690869844545,-87.6943432170782,-86.6978165896114,-85.773950742173),
 .UNSPECIFIED.);
#310=B_SPLINE_CURVE_WITH_KNOTS('',3,(#27676,#27677,#27678,#27679,#27680,
#27681,#27682,#27683,#27684,#27685,#27686,#27687,#27688,#27689,#27690,#27691,
#27692,#27693,#27694,#27695,#27696,#27697),.UNSPECIFIED.,.F.,.F.,(4,3,3,
3,3,3,3,4),(82.7956000313641,83.7082367072111,84.7047633346779,85.7012899621447,
86.6978165896115,87.6943432170783,88.690869844545,89.0787853385437),
 .UNSPECIFIED.);
#311=B_SPLINE_CURVE_WITH_KNOTS('',3,(#27702,#27703,#27704,#27705,#27706,
#27707,#27708,#27709,#27710,#27711,#27712,#27713,#27714,#27715,#27716,#27717,
#27718,#27719,#27720,#27721,#27722,#27723),.UNSPECIFIED.,.F.,.F.,(4,3,3,
3,3,3,3,4),(-98.3403213565322,-97.6596094917462,-96.6630828642794,-95.6665562368126,
-94.6700296093458,-93.673502981879,-92.6769763544122,-92.0571360493526),
 .UNSPECIFIED.);
#312=B_SPLINE_CURVE_WITH_KNOTS('',3,(#27724,#27725,#27726,#27727,#27728,
#27729,#27730,#27731,#27732,#27733,#27734,#27735,#27736,#27737,#27738,#27739,
#27740,#27741,#27742,#27743,#27744,#27745),.UNSPECIFIED.,.F.,.F.,(4,3,3,
3,3,3,3,4),(89.0787853385437,89.6873964720119,90.6839230994786,91.6804497269455,
92.6769763544122,93.673502981879,94.6700296093458,95.3619706457233),
 .UNSPECIFIED.);
#313=B_SPLINE_CURVE_WITH_KNOTS('',3,(#27750,#27751,#27752,#27753,#27754,
#27755,#27756,#27757,#27758,#27759,#27760,#27761,#27762,#27763,#27764,#27765,
#27766,#27767,#27768,#27769,#27770,#27771),.UNSPECIFIED.,.F.,.F.,(4,3,3,
3,3,3,3,4),(-104.623506663712,-103.638769256547,-102.64224262908,-101.645716001613,
-100.649189374147,-99.6526627466798,-98.656136119213,-98.3403213565322),
 .UNSPECIFIED.);
#314=B_SPLINE_CURVE_WITH_KNOTS('',3,(#27772,#27773,#27774,#27775,#27776,
#27777,#27778,#27779,#27780,#27781,#27782,#27783,#27784,#27785,#27786,#27787,
#27788,#27789,#27790,#27791,#27792,#27793),.UNSPECIFIED.,.F.,.F.,(4,3,3,
3,3,3,3,4),(95.3619706457233,95.6665562368126,96.6630828642794,97.6596094917462,
98.656136119213,99.6526627466798,100.649189374147,101.645155952903),
 .UNSPECIFIED.);
#315=B_SPLINE_CURVE_WITH_KNOTS('',3,(#27798,#27799,#27800,#27801,#27802,
#27803,#27804,#27805,#27806,#27807,#27808,#27809,#27810,#27811,#27812,#27813,
#27814,#27815,#27816,#27817,#27818,#27819,#27820,#27821,#27822),
 .UNSPECIFIED.,.F.,.F.,(4,3,3,3,3,3,3,3,4),(-110.906691970891,-110.614455648815,
-109.617929021348,-108.621402393881,-107.624875766414,-106.628349138947,
-105.631822511481,-104.635295884014,-104.623506663712),.UNSPECIFIED.);
#316=B_SPLINE_CURVE_WITH_KNOTS('',3,(#27823,#27824,#27825,#27826,#27827,
#27828,#27829,#27830,#27831,#27832,#27833,#27834,#27835,#27836,#27837,#27838,
#27839,#27840,#27841,#27842,#27843,#27844),.UNSPECIFIED.,.F.,.F.,(4,3,3,
3,3,3,3,4),(101.645155952903,102.64224262908,103.638769256547,104.635295884014,
105.631822511481,106.628349138947,107.624875766414,107.928341260083),
 .UNSPECIFIED.);
#317=B_SPLINE_CURVE_WITH_KNOTS('',3,(#27849,#27850,#27851,#27852,#27853,
#27854,#27855,#27856,#27857,#27858,#27859,#27860,#27861,#27862,#27863,#27864,
#27865,#27866,#27867,#27868,#27869,#27870),.UNSPECIFIED.,.F.,.F.,(4,3,3,
3,3,3,3,4),(-117.189877278071,-116.593615413615,-115.597088786149,-114.600562158682,
-113.604035531215,-112.607508903748,-111.610982276281,-110.906691970891),
 .UNSPECIFIED.);
#318=B_SPLINE_CURVE_WITH_KNOTS('',3,(#27871,#27872,#27873,#27874,#27875,
#27876,#27877,#27878,#27879,#27880,#27881,#27882,#27883,#27884,#27885,#27886,
#27887,#27888,#27889,#27890,#27891,#27892),.UNSPECIFIED.,.F.,.F.,(4,3,3,
3,3,3,3,4),(107.928341260083,108.621402393881,109.617929021348,110.614455648815,
111.610982276281,112.607508903748,113.604035531215,114.211526567262),
 .UNSPECIFIED.);
#319=B_SPLINE_CURVE_WITH_KNOTS('',3,(#27897,#27898,#27899,#27900,#27901,
#27902,#27903,#27904,#27905,#27906,#27907,#27908,#27909,#27910,#27911,#27912,
#27913,#27914,#27915,#27916,#27917,#27918),.UNSPECIFIED.,.F.,.F.,(4,3,3,
3,3,3,3,4),(-123.473062585251,-122.572775178416,-121.576248550949,-120.579721923483,
-119.583195296016,-118.586668668549,-117.590142041082,-117.189877278071),
 .UNSPECIFIED.);
#320=B_SPLINE_CURVE_WITH_KNOTS('',3,(#27919,#27920,#27921,#27922,#27923,
#27924,#27925,#27926,#27927,#27928,#27929,#27930,#27931,#27932,#27933,#27934,
#27935,#27936,#27937,#27938,#27939,#27940),.UNSPECIFIED.,.F.,.F.,(4,3,3,
3,3,3,3,4),(114.211526567262,114.600562158682,115.597088786149,116.593615413615,
117.590142041082,118.586668668549,119.583195296016,120.494711874442),
 .UNSPECIFIED.);
#321=B_SPLINE_CURVE_WITH_KNOTS('',3,(#27945,#27946,#27947,#27948,#27949,
#27950,#27951,#27952,#27953,#27954,#27955,#27956,#27957,#27958,#27959,#27960,
#27961,#27962,#27963,#27964,#27965,#27966,#27967,#27968,#27969),
 .UNSPECIFIED.,.F.,.F.,(4,3,3,3,3,3,3,3,4),(-129.75624789243,-129.548461570684,
-128.551934943217,-127.55540831575,-126.558881688283,-125.562355060817,
-124.56582843335,-123.569301805883,-123.473062585251),.UNSPECIFIED.);
#322=B_SPLINE_CURVE_WITH_KNOTS('',3,(#27970,#27971,#27972,#27973,#27974,
#27975,#27976,#27977,#27978,#27979,#27980,#27981,#27982,#27983,#27984,#27985,
#27986,#27987,#27988,#27989,#27990,#27991,#27992,#27993,#27994),
 .UNSPECIFIED.,.F.,.F.,(4,3,3,3,3,3,3,3,4),(120.494711874442,120.579721923483,
121.576248550949,122.572775178416,123.569301805883,124.56582843335,125.562355060817,
126.558881688283,126.777897181621),.UNSPECIFIED.);
#323=B_SPLINE_CURVE_WITH_KNOTS('',3,(#27999,#28000,#28001,#28002,#28003,
#28004,#28005,#28006,#28007,#28008,#28009,#28010,#28011,#28012,#28013,#28014,
#28015,#28016,#28017,#28018,#28019,#28020),.UNSPECIFIED.,.F.,.F.,(4,3,3,
3,3,3,3,4),(-136.03943319961,-135.527621335485,-134.531094708018,-133.534568080551,
-132.538041453084,-131.541514825617,-130.544988198151,-129.75624789243),
 .UNSPECIFIED.);
#324=B_SPLINE_CURVE_WITH_KNOTS('',3,(#28021,#28022,#28023,#28024,#28025,
#28026,#28027,#28028,#28029,#28030,#28031,#28032,#28033,#28034,#28035,#28036,
#28037,#28038,#28039,#28040,#28041,#28042),.UNSPECIFIED.,.F.,.F.,(4,3,3,
3,3,3,3,4),(126.777897181621,127.55540831575,128.551934943217,129.548461570684,
130.544988198151,131.541514825617,132.538041453084,133.061082488801),
 .UNSPECIFIED.);
#325=B_SPLINE_CURVE_WITH_KNOTS('',3,(#28047,#28048,#28049,#28050,#28051,
#28052,#28053,#28054,#28055,#28056,#28057,#28058,#28059,#28060,#28061,#28062,
#28063,#28064,#28065,#28066,#28067,#28068),.UNSPECIFIED.,.F.,.F.,(4,3,3,
3,3,3,3,4),(-142.322618506789,-141.506781100285,-140.510254472819,-139.513727845352,
-138.517201217885,-137.520674590418,-136.524147962951,-136.03943319961),
 .UNSPECIFIED.);
#326=B_SPLINE_CURVE_WITH_KNOTS('',3,(#28069,#28070,#28071,#28072,#28073,
#28074,#28075,#28076,#28077,#28078,#28079,#28080,#28081,#28082,#28083,#28084,
#28085,#28086,#28087,#28088,#28089,#28090),.UNSPECIFIED.,.F.,.F.,(4,3,3,
3,3,3,3,4),(133.061082488801,133.534568080551,134.531094708018,135.527621335485,
136.524147962951,137.520674590418,138.517201217885,139.34426779598),
 .UNSPECIFIED.);
#327=B_SPLINE_CURVE_WITH_KNOTS('',3,(#28096,#28097,#28098,#28099,#28100,
#28101,#28102,#28103),.UNSPECIFIED.,.F.,.F.,(4,1,1,1,1,4),(147.65485471872,
148.139569482062,149.136096109529,150.132622736996,151.129149364462,152.053589113585),
 .UNSPECIFIED.);
#328=B_SPLINE_CURVE_WITH_KNOTS('',3,(#28106,#28107,#28108,#28109,#28110,
#28111,#28112),.UNSPECIFIED.,.F.,.F.,(4,1,1,1,4),(147.65485471872,147.824314768092,
148.820841395558,149.817368023025,150.813894650492),.UNSPECIFIED.);
#329=B_SPLINE_CURVE_WITH_KNOTS('',3,(#28117,#28118,#28119,#28120,#28121,
#28122,#28123,#28124,#28125,#28126),.UNSPECIFIED.,.F.,.F.,(4,1,1,1,1,1,
1,4),(141.371669411541,142.160409717261,143.156936344728,144.153462972195,
145.149989599662,146.146516227128,147.143042854595,147.65485471872),
 .UNSPECIFIED.);
#330=B_SPLINE_CURVE_WITH_KNOTS('',3,(#28127,#28128,#28129,#28130,#28131,
#28132,#28133,#28134,#28135,#28136),.UNSPECIFIED.,.F.,.F.,(4,1,1,1,1,1,
1,4),(141.371669411541,141.845155003291,142.841681630758,143.838208258224,
144.834734885691,145.831261513158,146.827788140625,147.65485471872),
 .UNSPECIFIED.);
#331=B_SPLINE_CURVE_WITH_KNOTS('',3,(#28141,#28142,#28143,#28144,#28145,
#28146,#28147,#28148,#28149,#28150,#28151),.UNSPECIFIED.,.F.,.F.,(4,1,1,
1,1,1,1,1,4),(135.088484104361,135.184723324994,136.18124995246,137.177776579927,
138.174303207394,139.170829834861,140.167356462328,141.163883089794,141.371669411541),
 .UNSPECIFIED.);
#332=B_SPLINE_CURVE_WITH_KNOTS('',3,(#28152,#28153,#28154,#28155,#28156,
#28157,#28158,#28159,#28160,#28161),.UNSPECIFIED.,.F.,.F.,(4,1,1,1,1,1,
1,4),(135.088484104361,135.86599523849,136.862521865957,137.859048493424,
138.85557512089,139.852101748357,140.848628375824,141.371669411541),
 .UNSPECIFIED.);
#333=B_SPLINE_CURVE_WITH_KNOTS('',3,(#28166,#28167,#28168,#28169,#28170,
#28171,#28172,#28173,#28174,#28175),.UNSPECIFIED.,.F.,.F.,(4,1,1,1,1,1,
1,4),(128.805298797182,129.205563560193,130.20209018766,131.198616815126,
132.195143442593,133.19167007006,134.188196697527,135.088484104361),
 .UNSPECIFIED.);
#334=B_SPLINE_CURVE_WITH_KNOTS('',3,(#28176,#28177,#28178,#28179,#28180,
#28181,#28182,#28183,#28184,#28185,#28186),.UNSPECIFIED.,.F.,.F.,(4,1,1,
1,1,1,1,1,4),(128.805298797182,128.890308846222,129.886835473689,130.883362101156,
131.879888728623,132.87641535609,133.872941983556,134.869468611023,135.088484104361),
 .UNSPECIFIED.);
#335=B_SPLINE_CURVE_WITH_KNOTS('',3,(#28191,#28192,#28193,#28194,#28195,
#28196,#28197,#28198,#28199,#28200),.UNSPECIFIED.,.F.,.F.,(4,1,1,1,1,1,
1,4),(122.522113490002,123.226403795392,124.222930422859,125.219457050326,
126.215983677792,127.212510305259,128.209036932726,128.805298797182),
 .UNSPECIFIED.);
#336=B_SPLINE_CURVE_WITH_KNOTS('',3,(#28201,#28202,#28203,#28204,#28205,
#28206,#28207,#28208,#28209,#28210),.UNSPECIFIED.,.F.,.F.,(4,1,1,1,1,1,
1,4),(122.522113490002,122.911149081422,123.907675708888,124.904202336355,
125.900728963822,126.897255591289,127.893782218756,128.805298797182),
 .UNSPECIFIED.);
#337=B_SPLINE_CURVE_WITH_KNOTS('',3,(#28215,#28216,#28217,#28218,#28219,
#28220,#28221,#28222,#28223,#28224,#28225),.UNSPECIFIED.,.F.,.F.,(4,1,1,
1,1,1,1,1,4),(116.238928182822,116.250717403124,117.247244030591,118.243770658058,
119.240297285525,120.236823912992,121.233350540458,122.229877167925,122.522113490002),
 .UNSPECIFIED.);
#338=B_SPLINE_CURVE_WITH_KNOTS('',3,(#28226,#28227,#28228,#28229,#28230,
#28231,#28232,#28233,#28234,#28235),.UNSPECIFIED.,.F.,.F.,(4,1,1,1,1,1,
1,4),(116.238928182822,116.931989316621,117.928515944088,118.925042571554,
119.921569199021,120.918095826488,121.914622453955,122.522113490002),
 .UNSPECIFIED.);
#339=B_SPLINE_CURVE_WITH_KNOTS('',3,(#28240,#28241,#28242,#28243,#28244,
#28245,#28246,#28247,#28248,#28249),.UNSPECIFIED.,.F.,.F.,(4,1,1,1,1,1,
1,4),(109.955742875643,110.271557638324,111.26808426579,112.264610893257,
113.261137520724,114.257664148191,115.254190775658,116.238928182822),
 .UNSPECIFIED.);
#340=B_SPLINE_CURVE_WITH_KNOTS('',3,(#28250,#28251,#28252,#28253,#28254,
#28255,#28256,#28257,#28258,#28259,#28260),.UNSPECIFIED.,.F.,.F.,(4,1,1,
1,1,1,1,1,4),(109.955742875643,109.956302924353,110.95282955182,111.949356179287,
112.945882806754,113.94240943422,114.938936061687,115.935462689154,116.238928182822),
 .UNSPECIFIED.);
#341=B_SPLINE_CURVE_WITH_KNOTS('',3,(#28265,#28266,#28267,#28268,#28269,
#28270,#28271,#28272,#28273,#28274),.UNSPECIFIED.,.F.,.F.,(4,1,1,1,1,1,
1,4),(103.672557568463,104.292397873523,105.28892450099,106.285451128456,
107.281977755923,108.27850438339,109.275031010857,109.955742875643),
 .UNSPECIFIED.);
#342=B_SPLINE_CURVE_WITH_KNOTS('',3,(#28275,#28276,#28277,#28278,#28279,
#28280,#28281,#28282,#28283,#28284),.UNSPECIFIED.,.F.,.F.,(4,1,1,1,1,1,
1,4),(103.672557568463,103.977143159552,104.973669787019,105.970196414486,
106.966723041953,107.96324966942,108.959776296886,109.955742875643),
 .UNSPECIFIED.);
#343=B_SPLINE_CURVE_WITH_KNOTS('',3,(#28289,#28290,#28291,#28292,#28293,
#28294,#28295,#28296,#28297,#28298),.UNSPECIFIED.,.F.,.F.,(4,1,1,1,1,1,
1,4),(97.3893722612836,98.313238108722,99.3097647361889,100.306291363656,
101.302817991122,102.299344618589,103.295871246056,103.672557568463),
 .UNSPECIFIED.);
#344=B_SPLINE_CURVE_WITH_KNOTS('',3,(#28299,#28300,#28301,#28302,#28303,
#28304,#28305,#28306,#28307,#28308),.UNSPECIFIED.,.F.,.F.,(4,1,1,1,1,1,
1,4),(97.3893722612836,97.9979833947516,98.9945100222184,99.9910366496852,
100.987563277152,101.984089904619,102.980616532086,103.672557568463),
 .UNSPECIFIED.);
#345=B_SPLINE_CURVE_WITH_KNOTS('',3,(#28313,#28314,#28315,#28316,#28317,
#28318,#28319,#28320,#28321,#28322,#28323),.UNSPECIFIED.,.F.,.F.,(4,1,1,
1,1,1,1,1,4),(91.106186954104,91.3375517164545,92.3340783439213,93.3306049713881,
94.3271315988549,95.3236582263217,96.3201848537885,97.3167114812553,97.3893722612836),
 .UNSPECIFIED.);
#346=B_SPLINE_CURVE_WITH_KNOTS('',3,(#28324,#28325,#28326,#28327,#28328,
#28329,#28330,#28331,#28332,#28333),.UNSPECIFIED.,.F.,.F.,(4,1,1,1,1,1,
1,4),(91.106186954104,92.0188236299508,93.0153502574176,94.0118768848844,
95.0084035123512,96.004930139818,97.0014567672848,97.3893722612836),
 .UNSPECIFIED.);
#347=B_SPLINE_CURVE_WITH_KNOTS('',3,(#28338,#28339,#28340,#28341,#28342,
#28343,#28344,#28345,#28346,#28347),.UNSPECIFIED.,.F.,.F.,(4,1,1,1,1,1,
1,4),(84.8230016469244,85.3583919516537,86.3549185791205,87.3514452065873,
88.3479718340541,89.3444984615209,90.3410250889877,91.106186954104),
 .UNSPECIFIED.);
#348=B_SPLINE_CURVE_WITH_KNOTS('',3,(#28348,#28349,#28350,#28351,#28352,
#28353,#28354,#28355,#28356,#28357,#28358),.UNSPECIFIED.,.F.,.F.,(4,1,1,
1,1,1,1,1,4),(84.8230016469244,85.0431372376832,86.03966386515,87.0361904926168,
88.0327171200836,89.0292437475504,90.0257703750172,91.022297002484,91.106186954104),
 .UNSPECIFIED.);
#349=B_SPLINE_CURVE_WITH_KNOTS('',3,(#28363,#28364,#28365,#28366,#28367,
#28368,#28369,#28370,#28371,#28372),.UNSPECIFIED.,.F.,.F.,(4,1,1,1,1,1,
1,4),(78.5398163397449,79.3792321868529,80.3757588143197,81.3722854417865,
82.3688120692533,83.3653386967201,84.3618653241869,84.8230016469244),
 .UNSPECIFIED.);
#350=B_SPLINE_CURVE_WITH_KNOTS('',3,(#28373,#28374,#28375,#28376,#28377,
#28378,#28379,#28380,#28381,#28382),.UNSPECIFIED.,.F.,.F.,(4,1,1,1,1,1,
1,4),(78.5398163397449,79.0639774728824,80.0605041003492,81.057030727816,
82.0535573552828,83.0500839827496,84.0466106102164,84.8230016469244),
 .UNSPECIFIED.);
#351=B_SPLINE_CURVE_WITH_KNOTS('',3,(#28387,#28388,#28389,#28390,#28391,
#28392,#28393,#28394,#28395,#28396,#28397),.UNSPECIFIED.,.F.,.F.,(4,1,1,
1,1,1,1,1,4),(72.2566310325653,72.4035457945853,73.4000724220521,74.3965990495189,
75.3931256769857,76.3896523044525,77.3861789319193,78.3827055593861,78.5398163397449),
 .UNSPECIFIED.);
#352=B_SPLINE_CURVE_WITH_KNOTS('',3,(#28398,#28399,#28400,#28401,#28402,
#28403,#28404,#28405,#28406,#28407),.UNSPECIFIED.,.F.,.F.,(4,1,1,1,1,1,
1,4),(72.2566310325653,73.0848177080817,74.0813443355485,75.0778709630153,
76.0743975904821,77.0709242179488,78.0674508454156,78.5398163397449),
 .UNSPECIFIED.);
#353=B_SPLINE_CURVE_WITH_KNOTS('',3,(#28412,#28413,#28414,#28415,#28416,
#28417,#28418,#28419,#28420,#28421),.UNSPECIFIED.,.F.,.F.,(4,1,1,1,1,1,
1,4),(65.9734457253856,66.4243860297845,67.4209126572513,68.4174392847181,
69.4139659121849,70.4104925396517,71.4070191671185,72.2566310325653),
 .UNSPECIFIED.);
#354=B_SPLINE_CURVE_WITH_KNOTS('',3,(#28422,#28423,#28424,#28425,#28426,
#28427,#28428,#28429,#28430,#28431,#28432),.UNSPECIFIED.,.F.,.F.,(4,1,1,
1,1,1,1,1,4),(65.9734457253856,66.1091313158141,67.1056579432809,68.1021845707477,
69.0987111982145,70.0952378256813,71.0917644531481,72.0882910806149,72.2566310325653),
 .UNSPECIFIED.);
#355=B_SPLINE_CURVE_WITH_KNOTS('',3,(#28437,#28438,#28439,#28440,#28441,
#28442,#28443,#28444,#28445,#28446),.UNSPECIFIED.,.F.,.F.,(4,1,1,1,1,1,
1,4),(59.6902604182061,60.4452262649837,61.4417528924505,62.4382795199173,
63.4348061473841,64.4313327748509,65.4278594023177,65.9734457253856),
 .UNSPECIFIED.);
#356=B_SPLINE_CURVE_WITH_KNOTS('',3,(#28447,#28448,#28449,#28450,#28451,
#28452,#28453,#28454,#28455,#28456),.UNSPECIFIED.,.F.,.F.,(4,1,1,1,1,1,
1,4),(59.6902604182061,60.1299715510133,61.1264981784801,62.1230248059469,
63.1195514334137,64.1160780608805,65.1126046883473,65.9734457253856),
 .UNSPECIFIED.);
#357=B_SPLINE_CURVE_WITH_KNOTS('',3,(#28461,#28462,#28463,#28464,#28465,
#28466,#28467,#28468,#28469,#28470,#28471),.UNSPECIFIED.,.F.,.F.,(4,1,1,
1,1,1,1,1,4),(53.4070751110265,53.4695398727161,54.4660665001829,55.4625931276497,
56.4591197551165,57.4556463825833,58.4521730100501,59.4486996375169,59.6902604182061),
 .UNSPECIFIED.);
#358=B_SPLINE_CURVE_WITH_KNOTS('',3,(#28472,#28473,#28474,#28475,#28476,
#28477,#28478,#28479,#28480,#28481),.UNSPECIFIED.,.F.,.F.,(4,1,1,1,1,1,
1,4),(53.4070751110265,54.1508117862125,55.1473384136793,56.1438650411461,
57.1403916686129,58.1369182960797,59.1334449235465,59.6902604182061),
 .UNSPECIFIED.);
#359=B_SPLINE_CURVE_WITH_KNOTS('',3,(#28486,#28487,#28488,#28489,#28490,
#28491,#28492,#28493,#28494,#28495),.UNSPECIFIED.,.F.,.F.,(4,1,1,1,1,1,
1,4),(47.1238898038469,47.4903801079154,48.4869067353822,49.483433362849,
50.4799599903158,51.4764866177826,52.4730132452493,53.4070751110265),
 .UNSPECIFIED.);
#360=B_SPLINE_CURVE_WITH_KNOTS('',3,(#28496,#28497,#28498,#28499,#28500,
#28501,#28502,#28503,#28504,#28505,#28506),.UNSPECIFIED.,.F.,.F.,(4,1,1,
1,1,1,1,1,4),(47.1238898038469,47.1751253939449,48.1716520214117,49.1681786488785,
50.1647052763453,51.1612319038121,52.1577585312789,53.1542851587457,53.4070751110265),
 .UNSPECIFIED.);
#361=B_SPLINE_CURVE_WITH_KNOTS('',3,(#28511,#28512,#28513,#28514,#28515,
#28516,#28517,#28518,#28519,#28520),.UNSPECIFIED.,.F.,.F.,(4,1,1,1,1,1,
1,4),(40.8407044966673,41.5112203431146,42.5077469705814,43.5042735980482,
44.500800225515,45.4973268529818,46.4938534804486,47.1238898038469),
 .UNSPECIFIED.);
#362=B_SPLINE_CURVE_WITH_KNOTS('',3,(#28521,#28522,#28523,#28524,#28525,
#28526,#28527,#28528,#28529,#28530),.UNSPECIFIED.,.F.,.F.,(4,1,1,1,1,1,
1,4),(40.8407044966673,41.1959656291441,42.1924922566109,43.1890188840777,
44.1855455115445,45.1820721390113,46.1785987664781,47.1238898038469),
 .UNSPECIFIED.);
#363=B_SPLINE_CURVE_WITH_KNOTS('',3,(#28535,#28536,#28537,#28538,#28539,
#28540,#28541,#28542,#28543,#28544),.UNSPECIFIED.,.F.,.F.,(4,1,1,1,1,1,
1,4),(34.5575191894877,35.5320605783138,36.5285872057806,37.5251138332474,
38.5216404607142,39.518167088181,40.5146937156478,40.8407044966673),
 .UNSPECIFIED.);
#364=B_SPLINE_CURVE_WITH_KNOTS('',3,(#28545,#28546,#28547,#28548,#28549,
#28550,#28551,#28552,#28553,#28554),.UNSPECIFIED.,.F.,.F.,(4,1,1,1,1,1,
1,4),(34.5575191894877,35.2168058643433,36.2133324918101,37.2098591192769,
38.2063857467437,39.2029123742105,40.1994390016773,40.8407044966673),
 .UNSPECIFIED.);
#365=B_SPLINE_CURVE_WITH_KNOTS('',3,(#28559,#28560,#28561,#28562,#28563,
#28564,#28565,#28566,#28567,#28568,#28569),.UNSPECIFIED.,.F.,.F.,(4,1,1,
1,1,1,1,1,4),(28.2743338823081,28.5563741860462,29.552900813513,30.5494274409798,
31.5459540684466,32.5424806959134,33.5390073233802,34.535533950847,34.5575191894877),
 .UNSPECIFIED.);
#366=B_SPLINE_CURVE_WITH_KNOTS('',3,(#28570,#28571,#28572,#28573,#28574,
#28575,#28576,#28577,#28578,#28579),.UNSPECIFIED.,.F.,.F.,(4,1,1,1,1,1,
1,4),(28.2743338823081,29.2376460995425,30.2341727270093,31.2306993544761,
32.2272259819429,33.2237526094097,34.2202792368765,34.5575191894877),
 .UNSPECIFIED.);
#367=B_SPLINE_CURVE_WITH_KNOTS('',3,(#28584,#28585,#28586,#28587,#28588,
#28589,#28590,#28591,#28592,#28593),.UNSPECIFIED.,.F.,.F.,(4,1,1,1,1,1,
1,4),(21.9911485751285,22.5772144212454,23.5737410487122,24.570267676179,
25.5667943036458,26.5633209311126,27.5598475585794,28.2743338823081),
 .UNSPECIFIED.);
#368=B_SPLINE_CURVE_WITH_KNOTS('',3,(#28594,#28595,#28596,#28597,#28598,
#28599,#28600,#28601,#28602,#28603,#28604),.UNSPECIFIED.,.F.,.F.,(4,1,1,
1,1,1,1,1,4),(21.9911485751285,22.2619597072749,23.2584863347417,24.2550129622085,
25.2515395896753,26.2480662171421,27.2445928446089,28.2411194720757,28.2743338823081),
 .UNSPECIFIED.);
#369=B_SPLINE_CURVE_WITH_KNOTS('',3,(#28609,#28610,#28611,#28612,#28613,
#28614,#28615,#28616,#28617,#28618),.UNSPECIFIED.,.F.,.F.,(4,1,1,1,1,1,
1,4),(15.7079632679489,16.5980546564446,17.5945812839114,18.5911079113782,
19.587634538845,20.5841611663118,21.5806877937786,21.9911485751285),
 .UNSPECIFIED.);
#370=B_SPLINE_CURVE_WITH_KNOTS('',3,(#28619,#28620,#28621,#28622,#28623,
#28624,#28625,#28626,#28627,#28628),.UNSPECIFIED.,.F.,.F.,(4,1,1,1,1,1,
1,4),(15.7079632679489,16.2827999424742,17.279326569941,18.2758531974078,
19.2723798248745,20.2689064523413,21.2654330798081,21.9911485751285),
 .UNSPECIFIED.);
#371=B_SPLINE_CURVE_WITH_KNOTS('',3,(#29214,#29215,#29216,#29217,#29218,
#29219,#29220,#29221,#29222,#29223,#29224,#29225,#29226,#29227,#29228,#29229,
#29230,#29231,#29232,#29233,#29234,#29235,#29236,#29237,#29238,#29239,#29240,
#29241,#29242,#29243,#29244,#29245,#29246,#29247,#29248,#29249,#29250,#29251,
#29252,#29253,#29254,#29255,#29256,#29257,#29258,#29259,#29260,#29261,#29262,
#29263,#29264,#29265,#29266,#29267,#29268,#29269,#29270,#29271,#29272,#29273,
#29274,#29275,#29276,#29277,#29278,#29279,#29280,#29281,#29282,#29283,#29284,
#29285,#29286,#29287,#29288,#29289,#29290,#29291,#29292,#29293,#29294,#29295,
#29296,#29297,#29298),.UNSPECIFIED.,.F.,.F.,(4,3,3,3,3,3,3,3,3,3,3,3,3,
3,3,3,3,3,3,3,3,3,3,3,3,3,3,3,4),(-0.364629307890647,-0.350570973320307,
-0.328978052818744,-0.318517199510329,-0.314077304067069,-0.309443350704567,
-0.288121479269547,-0.272860168701457,-0.264083461271192,-0.260314272498768,
-0.239583028334462,-0.219361432489358,-0.206028823048227,-0.194764789032429,
-0.191353184809912,-0.171767825397509,-0.166030994724833,-0.145277120384229,
-0.126464847198481,-0.122930812072354,-0.103474254747116,-0.0841030460574836,
-0.065133557541488,-0.0617046221863798,-0.0585874619642264,-0.0400020264087737,
-0.0217528946302394,-0.00408444113370017,0.),.UNSPECIFIED.);
#372=B_SPLINE_CURVE_WITH_KNOTS('',3,(#29299,#29300,#29301,#29302,#29303,
#29304,#29305),.UNSPECIFIED.,.F.,.F.,(4,3,4),(139.34426779598,139.513727845352,
140.438167594474),.UNSPECIFIED.);
#373=B_SPLINE_CURVE_WITH_KNOTS('',3,(#29307,#29308,#29309,#29310,#29311,
#29312,#29313,#29314,#29315,#29316,#29317,#29318,#29319,#29320,#29321,#29322,
#29323,#29324,#29325,#29326,#29327,#29328,#29329,#29330,#29331,#29332,#29333,
#29334,#29335,#29336,#29337,#29338,#29339,#29340,#29341,#29342,#29343,#29344,
#29345,#29346,#29347,#29348,#29349,#29350,#29351,#29352,#29353,#29354,#29355,
#29356,#29357,#29358,#29359,#29360,#29361,#29362,#29363,#29364,#29365,#29366,
#29367,#29368,#29369,#29370,#29371,#29372,#29373,#29374,#29375,#29376,#29377,
#29378,#29379,#29380,#29381,#29382,#29383,#29384,#29385,#29386,#29387,#29388,
#29389,#29390,#29391,#29392,#29393,#29394),.UNSPECIFIED.,.F.,.F.,(4,3,3,
3,3,3,3,3,3,3,3,3,3,3,3,3,3,3,3,3,3,3,3,3,3,3,3,3,3,4),(-0.366397579005848,
-0.354990427718542,-0.337010231564958,-0.326410787528287,-0.321616430488346,
-0.302809998808161,-0.288326910148396,-0.283342059075868,-0.278582852742593,
-0.25916977354628,-0.239351473889624,-0.226249927799729,-0.21981438558208,
-0.215722421417741,-0.212569226271925,-0.19213662083836,-0.186945289530043,
-0.167235228589776,-0.156543539884273,-0.148369952063709,-0.143888792518516,
-0.123411612445278,-0.102503519065178,-0.081437114422489,-0.0761190075298889,
-0.072239458013529,-0.0505972726117569,-0.0289036910298352,-0.0076720951992491,
0.),.UNSPECIFIED.);
#374=B_SPLINE_CURVE_WITH_KNOTS('',3,(#29395,#29396,#29397,#29398,#29399,
#29400,#29401,#29402,#29403),.UNSPECIFIED.,.F.,.F.,(4,1,1,1,1,1,4),(10.3757270560179,
11.3001668051402,12.296693432607,13.2932200600738,14.2897466875406,15.2862733150074,
15.7079632679489),.UNSPECIFIED.);
#375=B_SPLINE_CURVE_WITH_KNOTS('',3,(#29409,#29410,#29411,#29412,#29413,
#29414,#29415,#29416,#29417,#29418,#29419,#29420,#29421,#29422,#29423,#29424,
#29425,#29426,#29427,#29428,#29429,#29430,#29431,#29432,#29433,#29434,#29435,
#29436,#29437,#29438,#29439,#29440,#29441,#29442,#29443,#29444,#29445,#29446,
#29447,#29448,#29449,#29450,#29451,#29452,#29453,#29454,#29455,#29456,#29457,
#29458,#29459,#29460,#29461,#29462,#29463,#29464,#29465,#29466,#29467,#29468,
#29469,#29470,#29471,#29472,#29473,#29474,#29475,#29476,#29477,#29478,#29479,
#29480,#29481,#29482,#29483,#29484,#29485,#29486,#29487,#29488,#29489,#29490,
#29491,#29492,#29493),.UNSPECIFIED.,.F.,.F.,(4,3,3,3,3,3,3,3,3,3,3,3,3,
3,3,3,3,3,3,3,3,3,3,3,3,3,3,3,4),(-0.364629307890666,-0.350570973320324,
-0.328978052669231,-0.318517197828435,-0.314077299887452,-0.309443349083419,
-0.288121477417662,-0.272860167081056,-0.264083457003318,-0.260314270665685,
-0.239583025704171,-0.219361424327907,-0.206028816927134,-0.194764778888859,
-0.191353179101175,-0.171767814271692,-0.166030994724817,-0.145277120384215,
-0.126464843813837,-0.122930811559716,-0.103474253035366,-0.0841030482674331,
-0.0651335676695573,-0.0617046646810245,-0.0585874714057973,-0.0400020414921941,
-0.0217529178875472,-0.00408447427804078,0.),.UNSPECIFIED.);
#376=B_SPLINE_CURVE_WITH_KNOTS('',3,(#29496,#29497,#29498,#29499,#29500,
#29501,#29502,#29503),.UNSPECIFIED.,.F.,.F.,(4,1,1,1,1,4),(11.6154215191106,
12.6119481465774,13.6084747740442,14.605001401511,15.6015280289778,15.7079632679489),
 .UNSPECIFIED.);
#377=B_SPLINE_CURVE_WITH_KNOTS('',3,(#30089,#30090,#30091,#30092,#30093,
#30094,#30095,#30096,#30097,#30098,#30099,#30100,#30101,#30102,#30103,#30104,
#30105,#30106,#30107,#30108,#30109,#30110,#30111,#30112,#30113,#30114,#30115,
#30116,#30117,#30118,#30119,#30120,#30121,#30122,#30123,#30124,#30125,#30126,
#30127,#30128,#30129,#30130,#30131,#30132,#30133,#30134,#30135,#30136,#30137,
#30138,#30139,#30140,#30141,#30142,#30143,#30144,#30145,#30146,#30147,#30148,
#30149,#30150,#30151,#30152,#30153,#30154,#30155,#30156,#30157,#30158,#30159,
#30160,#30161,#30162,#30163,#30164,#30165,#30166,#30167,#30168,#30169,#30170,
#30171,#30172,#30173,#30174,#30175,#30176),.UNSPECIFIED.,.F.,.F.,(4,3,3,
3,3,3,3,3,3,3,3,3,3,3,3,3,3,3,3,3,3,3,3,3,3,3,3,3,3,4),(-0.366397579005786,
-0.354990427718483,-0.337010225011654,-0.326410775254011,-0.321616427612408,
-0.302809991569146,-0.288326903814256,-0.283342034586426,-0.278582850271486,
-0.259169767533232,-0.239351468146884,-0.226249923492668,-0.219814377104185,
-0.215722361896418,-0.212569123121559,-0.192136517860909,-0.18694528953002,
-0.167235226419274,-0.156543536652707,-0.148369941282216,-0.143888792324927,
-0.123411609583119,-0.102503513459085,-0.0814371085565346,-0.0761189992864274,
-0.0722394608782654,-0.0505972736076427,-0.0289036933900785,-0.00767210533094177,
0.),.UNSPECIFIED.);
#378=B_SPLINE_CURVE_WITH_KNOTS('',3,(#30177,#30178,#30179,#30180),
 .UNSPECIFIED.,.F.,.F.,(4,4),(-142.503307727752,-142.322618506789),
 .UNSPECIFIED.);
#379=B_SPLINE_CURVE_WITH_KNOTS('',3,(#30252,#30253,#30254,#30255,#30256,
#30257,#30258,#30259,#30260,#30261),.UNSPECIFIED.,.F.,.F.,(4,3,3,4),(-4.09254174883827,
-3.98675360377158,-2.99006520282869,-2.06514013327809),.UNSPECIFIED.);
#380=B_SPLINE_CURVE_WITH_KNOTS('',3,(#30264,#30265,#30266,#30267,#30268,
#30269,#30270),.UNSPECIFIED.,.F.,.F.,(4,3,4),(0.,0.996688400942905,1.11419103802963),
 .UNSPECIFIED.);
#381=B_SPLINE_CURVE_WITH_KNOTS('',3,(#30275,#30276,#30277,#30278,#30279,
#30280,#30281,#30282,#30283,#30284,#30285,#30286,#30287,#30288,#30289,#30290,
#30291,#30292,#30293,#30294,#30295,#30296),.UNSPECIFIED.,.F.,.F.,(4,3,3,
3,3,3,3,4),(-10.3757270560179,-9.96688400942895,-8.97019560848606,-7.97350720754317,
-6.97681880660027,-5.98013040565738,-4.98344200471448,-4.09254174883827),
 .UNSPECIFIED.);
#382=B_SPLINE_CURVE_WITH_KNOTS('',3,(#30297,#30298,#30299,#30300,#30301,
#30302,#30303,#30304,#30305,#30306,#30307,#30308,#30309,#30310,#30311,#30312,
#30313,#30314,#30315,#30316,#30317,#30318),.UNSPECIFIED.,.F.,.F.,(4,3,3,
3,3,3,3,4),(1.11419103802963,1.9933768018858,2.99006520282869,3.98675360377159,
4.98344200471448,5.98013040565737,6.97681880660027,7.39737634520922),
 .UNSPECIFIED.);
#383=B_SPLINE_CURVE_WITH_KNOTS('',3,(#30323,#30324,#30325,#30326,#30327,
#30328,#30329,#30330,#30331,#30332,#30333,#30334,#30335,#30336,#30337,#30338,
#30339,#30340,#30341,#30342,#30343,#30344),.UNSPECIFIED.,.F.,.F.,(4,3,3,
3,3,3,3,4),(-16.6589123631975,-15.9470144150863,-14.9503260141434,-13.9536376132005,
-12.9569492122576,-11.9602608113147,-10.9635724103719,-10.3757270560179),
 .UNSPECIFIED.);
#384=B_SPLINE_CURVE_WITH_KNOTS('',3,(#30345,#30346,#30347,#30348,#30349,
#30350,#30351,#30352,#30353,#30354,#30355,#30356,#30357,#30358,#30359,#30360,
#30361,#30362,#30363,#30364,#30365,#30366),.UNSPECIFIED.,.F.,.F.,(4,3,3,
3,3,3,3,4),(7.39737634520922,7.97350720754316,8.97019560848606,9.96688400942896,
10.9635724103719,11.9602608113148,12.9569492122576,13.6805616523888),
 .UNSPECIFIED.);
#385=B_SPLINE_CURVE_WITH_KNOTS('',3,(#30371,#30372,#30373,#30374,#30375,
#30376,#30377,#30378,#30379,#30380,#30381,#30382,#30383,#30384,#30385,#30386,
#30387,#30388,#30389,#30390,#30391,#30392,#30393,#30394,#30395),
 .UNSPECIFIED.,.F.,.F.,(4,3,3,3,3,3,3,3,4),(-22.942097670377,-22.9238332216866,
-21.9271448207437,-20.9304564198008,-19.9337680188579,-18.937079617915,
-17.9403912169721,-16.9437028160292,-16.6589123631975),.UNSPECIFIED.);
#386=B_SPLINE_CURVE_WITH_KNOTS('',3,(#30396,#30397,#30398,#30399,#30400,
#30401,#30402,#30403,#30404,#30405,#30406,#30407,#30408,#30409,#30410,#30411,
#30412,#30413,#30414,#30415,#30416,#30417,#30418,#30419,#30420),
 .UNSPECIFIED.,.F.,.F.,(4,3,3,3,3,3,3,3,4),(13.6805616523888,13.9536376132005,
14.9503260141434,15.9470144150863,16.9437028160292,17.9403912169721,18.937079617915,
19.9337680188579,19.9637469595684),.UNSPECIFIED.);
#387=B_SPLINE_CURVE_WITH_KNOTS('',3,(#30425,#30426,#30427,#30428,#30429,
#30430,#30431,#30432,#30433,#30434,#30435,#30436,#30437,#30438,#30439,#30440,
#30441,#30442,#30443,#30444,#30445,#30446),.UNSPECIFIED.,.F.,.F.,(4,3,3,
3,3,3,3,4),(-29.2252829775566,-28.903963627344,-27.9072752264011,-26.9105868254582,
-25.9138984245153,-24.9172100235724,-23.9205216226295,-22.942097670377),
 .UNSPECIFIED.);
#388=B_SPLINE_CURVE_WITH_KNOTS('',3,(#30447,#30448,#30449,#30450,#30451,
#30452,#30453,#30454,#30455,#30456,#30457,#30458,#30459,#30460,#30461,#30462,
#30463,#30464,#30465,#30466,#30467,#30468),.UNSPECIFIED.,.F.,.F.,(4,3,3,
3,3,3,3,4),(19.9637469595684,20.9304564198008,21.9271448207437,22.9238332216866,
23.9205216226295,24.9172100235724,25.9138984245153,26.246932266748),
 .UNSPECIFIED.);
#389=B_SPLINE_CURVE_WITH_KNOTS('',3,(#30473,#30474,#30475,#30476,#30477,
#30478,#30479,#30480,#30481,#30482,#30483,#30484,#30485,#30486,#30487,#30488,
#30489,#30490,#30491,#30492,#30493,#30494),.UNSPECIFIED.,.F.,.F.,(4,3,3,
3,3,3,3,4),(-35.5084682847362,-34.8840940330013,-33.8874056320584,-32.8907172311156,
-31.8940288301727,-30.8973404292298,-29.9006520282869,-29.2252829775566),
 .UNSPECIFIED.);
#390=B_SPLINE_CURVE_WITH_KNOTS('',3,(#30495,#30496,#30497,#30498,#30499,
#30500,#30501,#30502,#30503,#30504,#30505,#30506,#30507,#30508,#30509,#30510,
#30511,#30512,#30513,#30514,#30515,#30516),.UNSPECIFIED.,.F.,.F.,(4,3,3,
3,3,3,3,4),(26.246932266748,26.9105868254582,27.9072752264011,28.903963627344,
29.9006520282869,30.8973404292298,31.8940288301727,32.5301175739276),
 .UNSPECIFIED.);
#391=B_SPLINE_CURVE_WITH_KNOTS('',3,(#30521,#30522,#30523,#30524,#30525,
#30526,#30527,#30528,#30529,#30530,#30531,#30532,#30533,#30534,#30535,#30536,
#30537,#30538,#30539,#30540,#30541,#30542),.UNSPECIFIED.,.F.,.F.,(4,3,3,
3,3,3,3,4),(-41.7916535919158,-40.8642244386587,-39.8675360377158,-38.8708476367729,
-37.87415923583,-36.8774708348871,-35.8807824339442,-35.5084682847362),
 .UNSPECIFIED.);
#392=B_SPLINE_CURVE_WITH_KNOTS('',3,(#30543,#30544,#30545,#30546,#30547,
#30548,#30549,#30550,#30551,#30552,#30553,#30554,#30555,#30556,#30557,#30558,
#30559,#30560,#30561,#30562,#30563,#30564),.UNSPECIFIED.,.F.,.F.,(4,3,3,
3,3,3,3,4),(32.5301175739276,32.8907172311156,33.8874056320585,34.8840940330014,
35.8807824339443,36.8774708348872,37.8741592358301,38.8133028811072),
 .UNSPECIFIED.);
#393=B_SPLINE_CURVE_WITH_KNOTS('',3,(#30569,#30570,#30571,#30572,#30573,
#30574,#30575,#30576,#30577,#30578,#30579,#30580,#30581,#30582,#30583,#30584,
#30585,#30586,#30587,#30588,#30589,#30590,#30591,#30592,#30593),
 .UNSPECIFIED.,.F.,.F.,(4,3,3,3,3,3,3,3,4),(-48.0748388990954,-47.841043245259,
-46.8443548443161,-45.8476664433732,-44.8509780424303,-43.8542896414874,
-42.8576012405445,-41.8609128396016,-41.7916535919158),.UNSPECIFIED.);
#394=B_SPLINE_CURVE_WITH_KNOTS('',3,(#30594,#30595,#30596,#30597,#30598,
#30599,#30600,#30601,#30602,#30603,#30604,#30605,#30606,#30607,#30608,#30609,
#30610,#30611,#30612,#30613,#30614,#30615,#30616,#30617,#30618),
 .UNSPECIFIED.,.F.,.F.,(4,3,3,3,3,3,3,3,4),(38.8133028811072,38.8708476367729,
39.8675360377158,40.8642244386587,41.8609128396016,42.8576012405445,43.8542896414874,
44.8509780424303,45.0964881882868),.UNSPECIFIED.);
#395=B_SPLINE_CURVE_WITH_KNOTS('',3,(#30623,#30624,#30625,#30626,#30627,
#30628,#30629,#30630,#30631,#30632,#30633,#30634,#30635,#30636,#30637,#30638,
#30639,#30640,#30641,#30642,#30643,#30644),.UNSPECIFIED.,.F.,.F.,(4,3,3,
3,3,3,3,4),(-54.358024206275,-53.8211736509164,-52.8244852499735,-51.8277968490306,
-50.8311084480877,-49.8344200471448,-48.8377316462019,-48.0748388990954),
 .UNSPECIFIED.);
#396=B_SPLINE_CURVE_WITH_KNOTS('',3,(#30645,#30646,#30647,#30648,#30649,
#30650,#30651,#30652,#30653,#30654,#30655,#30656,#30657,#30658,#30659,#30660,
#30661,#30662,#30663,#30664,#30665,#30666),.UNSPECIFIED.,.F.,.F.,(4,3,3,
3,3,3,3,4),(45.0964881882868,45.8476664433732,46.8443548443161,47.841043245259,
48.8377316462019,49.8344200471448,50.8311084480877,51.3796734954663),
 .UNSPECIFIED.);
#397=B_SPLINE_CURVE_WITH_KNOTS('',3,(#30671,#30672,#30673,#30674,#30675,
#30676,#30677,#30678,#30679,#30680,#30681,#30682,#30683,#30684,#30685,#30686,
#30687,#30688,#30689,#30690,#30691,#30692),.UNSPECIFIED.,.F.,.F.,(4,3,3,
3,3,3,3,4),(-60.6412095134546,-59.8013040565737,-58.8046156556308,-57.8079272546879,
-56.811238853745,-55.8145504528021,-54.8178620518593,-54.358024206275),
 .UNSPECIFIED.);
#398=B_SPLINE_CURVE_WITH_KNOTS('',3,(#30693,#30694,#30695,#30696,#30697,
#30698,#30699,#30700,#30701,#30702,#30703,#30704,#30705,#30706,#30707,#30708,
#30709,#30710,#30711,#30712,#30713,#30714),.UNSPECIFIED.,.F.,.F.,(4,3,3,
3,3,3,3,4),(51.3796734954663,51.8277968490306,52.8244852499735,53.8211736509164,
54.8178620518593,55.8145504528022,56.8112388537451,57.6628588026459),
 .UNSPECIFIED.);
#399=B_SPLINE_CURVE_WITH_KNOTS('',3,(#30719,#30720,#30721,#30722,#30723,
#30724,#30725,#30726,#30727,#30728,#30729,#30730,#30731,#30732,#30733,#30734,
#30735,#30736,#30737,#30738,#30739,#30740,#30741,#30742,#30743),
 .UNSPECIFIED.,.F.,.F.,(4,3,3,3,3,3,3,3,4),(-66.9243948206342,-66.778122863174,
-65.7814344622311,-64.7847460612882,-63.7880576603453,-62.7913692594024,
-61.7946808584595,-60.7979924575166,-60.6412095134546),.UNSPECIFIED.);
#400=B_SPLINE_CURVE_WITH_KNOTS('',3,(#30744,#30745,#30746,#30747,#30748,
#30749,#30750,#30751,#30752,#30753,#30754,#30755,#30756,#30757,#30758,#30759,
#30760,#30761,#30762,#30763,#30764,#30765,#30766,#30767,#30768),
 .UNSPECIFIED.,.F.,.F.,(4,3,3,3,3,3,3,3,4),(57.6628588026459,57.8079272546879,
58.8046156556308,59.8013040565737,60.7979924575166,61.7946808584595,62.7913692594024,
63.7880576603453,63.9460441098255),.UNSPECIFIED.);
#401=B_SPLINE_CURVE_WITH_KNOTS('',3,(#30773,#30774,#30775,#30776,#30777,
#30778,#30779,#30780,#30781,#30782,#30783,#30784,#30785,#30786,#30787,#30788,
#30789,#30790,#30791,#30792,#30793,#30794),.UNSPECIFIED.,.F.,.F.,(4,3,3,
3,3,3,3,4),(-73.2075801278138,-72.7582532688314,-71.7615648678885,-70.7648764669456,
-69.7681880660027,-68.7714996650598,-67.7748112641169,-66.9243948206342),
 .UNSPECIFIED.);
#402=B_SPLINE_CURVE_WITH_KNOTS('',3,(#30795,#30796,#30797,#30798,#30799,
#30800,#30801,#30802,#30803,#30804,#30805,#30806,#30807,#30808,#30809,#30810,
#30811,#30812,#30813,#30814,#30815,#30816),.UNSPECIFIED.,.F.,.F.,(4,3,3,
3,3,3,3,4),(63.9460441098255,64.7847460612882,65.7814344622311,66.778122863174,
67.7748112641169,68.7714996650598,69.7681880660027,70.2292294170051),
 .UNSPECIFIED.);
#403=B_SPLINE_CURVE_WITH_KNOTS('',3,(#30821,#30822,#30823,#30824,#30825,
#30826,#30827,#30828,#30829,#30830,#30831,#30832,#30833,#30834,#30835,#30836,
#30837,#30838,#30839,#30840,#30841,#30842),.UNSPECIFIED.,.F.,.F.,(4,3,3,
3,3,3,3,4),(-79.4907654349934,-78.7383836744887,-77.7416952735459,-76.745006872603,
-75.7483184716601,-74.7516300707172,-73.7549416697743,-73.2075801278138),
 .UNSPECIFIED.);
#404=B_SPLINE_CURVE_WITH_KNOTS('',3,(#30843,#30844,#30845,#30846,#30847,
#30848,#30849,#30850,#30851,#30852,#30853,#30854,#30855,#30856,#30857,#30858,
#30859,#30860,#30861,#30862,#30863,#30864),.UNSPECIFIED.,.F.,.F.,(4,3,3,
3,3,3,3,4),(70.2292294170051,70.7648764669456,71.7615648678885,72.7582532688314,
73.7549416697743,74.7516300707172,75.7483184716601,76.5124147241847),
 .UNSPECIFIED.);
#405=B_SPLINE_CURVE_WITH_KNOTS('',3,(#30869,#30870,#30871,#30872,#30873,
#30874,#30875,#30876,#30877,#30878,#30879,#30880,#30881,#30882,#30883,#30884,
#30885,#30886,#30887,#30888,#30889,#30890,#30891,#30892,#30893),
 .UNSPECIFIED.,.F.,.F.,(4,3,3,3,3,3,3,3,4),(-85.773950742173,-85.715202481089,
-84.7185140801461,-83.7218256792032,-82.7251372782603,-81.7284488773174,
-80.7317604763745,-79.7350720754316,-79.4907654349934),.UNSPECIFIED.);
#406=B_SPLINE_CURVE_WITH_KNOTS('',3,(#30894,#30895,#30896,#30897,#30898,
#30899,#30900,#30901,#30902,#30903,#30904,#30905,#30906,#30907,#30908,#30909,
#30910,#30911,#30912,#30913,#30914,#30915,#30916,#30917,#30918),
 .UNSPECIFIED.,.F.,.F.,(4,3,3,3,3,3,3,3,4),(76.5124147241847,76.745006872603,
77.7416952735459,78.7383836744888,79.7350720754317,80.7317604763746,81.7284488773175,
82.7251372782604,82.7956000313643),.UNSPECIFIED.);
#407=B_SPLINE_CURVE_WITH_KNOTS('',3,(#30923,#30924,#30925,#30926,#30927,
#30928,#30929,#30930,#30931,#30932,#30933,#30934,#30935,#30936,#30937,#30938,
#30939,#30940,#30941,#30942,#30943,#30944),.UNSPECIFIED.,.F.,.F.,(4,3,3,
3,3,3,3,4),(-92.0571360493526,-91.6953328867464,-90.6986444858035,-89.7019560848606,
-88.7052676839177,-87.7085792829748,-86.7118908820319,-85.773950742173),
 .UNSPECIFIED.);
#408=B_SPLINE_CURVE_WITH_KNOTS('',3,(#30945,#30946,#30947,#30948,#30949,
#30950,#30951,#30952,#30953,#30954,#30955,#30956,#30957,#30958,#30959,#30960,
#30961,#30962,#30963,#30964,#30965,#30966),.UNSPECIFIED.,.F.,.F.,(4,3,3,
3,3,3,3,4),(82.7956000313643,83.7218256792033,84.7185140801462,85.715202481089,
86.711890882032,87.7085792829748,88.7052676839177,89.0787853385439),
 .UNSPECIFIED.);
#409=B_SPLINE_CURVE_WITH_KNOTS('',3,(#30971,#30972,#30973,#30974,#30975,
#30976,#30977,#30978,#30979,#30980,#30981,#30982,#30983,#30984,#30985,#30986,
#30987,#30988,#30989,#30990,#30991,#30992),.UNSPECIFIED.,.F.,.F.,(4,3,3,
3,3,3,3,4),(-98.3403213565321,-97.6754632924037,-96.6787748914608,-95.682086490518,
-94.6853980895751,-93.6887096886322,-92.6920212876893,-92.0571360493526),
 .UNSPECIFIED.);
#410=B_SPLINE_CURVE_WITH_KNOTS('',3,(#30993,#30994,#30995,#30996,#30997,
#30998,#30999,#31000,#31001,#31002,#31003,#31004,#31005,#31006,#31007,#31008,
#31009,#31010,#31011,#31012,#31013,#31014),.UNSPECIFIED.,.F.,.F.,(4,3,3,
3,3,3,3,4),(89.0787853385439,89.7019560848606,90.6986444858035,91.6953328867464,
92.6920212876893,93.6887096886322,94.6853980895751,95.3619706457235),
 .UNSPECIFIED.);
#411=B_SPLINE_CURVE_WITH_KNOTS('',3,(#31019,#31020,#31021,#31022,#31023,
#31024,#31025,#31026,#31027,#31028,#31029,#31030,#31031,#31032,#31033,#31034,
#31035,#31036,#31037,#31038,#31039,#31040),.UNSPECIFIED.,.F.,.F.,(4,3,3,
3,3,3,3,4),(-104.623506663712,-103.655593698061,-102.658905297118,-101.662216896175,
-100.665528495232,-99.6688400942895,-98.6721516933466,-98.3403213565321),
 .UNSPECIFIED.);
#412=B_SPLINE_CURVE_WITH_KNOTS('',3,(#31041,#31042,#31043,#31044,#31045,
#31046,#31047,#31048,#31049,#31050,#31051,#31052,#31053,#31054,#31055,#31056,
#31057,#31058,#31059,#31060,#31061,#31062),.UNSPECIFIED.,.F.,.F.,(4,3,3,
3,3,3,3,4),(95.3619706457235,95.682086490518,96.6787748914609,97.6754632924038,
98.6721516933467,99.6688400942896,100.665528495232,101.645155952903),
 .UNSPECIFIED.);
#413=B_SPLINE_CURVE_WITH_KNOTS('',3,(#31067,#31068,#31069,#31070,#31071,
#31072,#31073,#31074,#31075,#31076,#31077,#31078,#31079,#31080,#31081,#31082,
#31083,#31084,#31085,#31086,#31087,#31088,#31089,#31090,#31091),
 .UNSPECIFIED.,.F.,.F.,(4,3,3,3,3,3,3,3,4),(-110.906691970891,-110.632412504661,
-109.635724103719,-108.639035702776,-107.642347301833,-106.64565890089,
-105.648970499947,-104.652282099004,-104.623506663712),.UNSPECIFIED.);
#414=B_SPLINE_CURVE_WITH_KNOTS('',3,(#31092,#31093,#31094,#31095,#31096,
#31097,#31098,#31099,#31100,#31101,#31102,#31103,#31104,#31105,#31106,#31107,
#31108,#31109,#31110,#31111,#31112,#31113,#31114,#31115,#31116),
 .UNSPECIFIED.,.F.,.F.,(4,3,3,3,3,3,3,3,4),(101.645155952903,101.662216896175,
102.658905297118,103.655593698061,104.652282099004,105.648970499947,106.64565890089,
107.642347301833,107.928341260083),.UNSPECIFIED.);
#415=B_SPLINE_CURVE_WITH_KNOTS('',3,(#31121,#31122,#31123,#31124,#31125,
#31126,#31127,#31128,#31129,#31130,#31131,#31132,#31133,#31134,#31135,#31136,
#31137,#31138,#31139,#31140,#31141,#31142),.UNSPECIFIED.,.F.,.F.,(4,3,3,
3,3,3,3,4),(-117.189877278071,-116.612542910319,-115.615854509376,-114.619166108433,
-113.62247770749,-112.625789306547,-111.629100905604,-110.906691970891),
 .UNSPECIFIED.);
#416=B_SPLINE_CURVE_WITH_KNOTS('',3,(#31143,#31144,#31145,#31146,#31147,
#31148,#31149,#31150,#31151,#31152,#31153,#31154,#31155,#31156,#31157,#31158,
#31159,#31160,#31161,#31162,#31163,#31164),.UNSPECIFIED.,.F.,.F.,(4,3,3,
3,3,3,3,4),(107.928341260083,108.639035702776,109.635724103719,110.632412504661,
111.629100905604,112.625789306547,113.62247770749,114.211526567262),
 .UNSPECIFIED.);
#417=B_SPLINE_CURVE_WITH_KNOTS('',3,(#31169,#31170,#31171,#31172,#31173,
#31174,#31175,#31176,#31177,#31178,#31179,#31180,#31181,#31182,#31183,#31184,
#31185,#31186,#31187,#31188,#31189,#31190),.UNSPECIFIED.,.F.,.F.,(4,3,3,
3,3,3,3,4),(-123.473062585251,-122.592673315976,-121.595984915033,-120.59929651409,
-119.602608113147,-118.605919712205,-117.609231311262,-117.189877278071),
 .UNSPECIFIED.);
#418=B_SPLINE_CURVE_WITH_KNOTS('',3,(#31191,#31192,#31193,#31194,#31195,
#31196,#31197,#31198,#31199,#31200,#31201,#31202,#31203,#31204,#31205,#31206,
#31207,#31208,#31209,#31210,#31211,#31212),.UNSPECIFIED.,.F.,.F.,(4,3,3,
3,3,3,3,4),(114.211526567262,114.619166108433,115.615854509376,116.612542910319,
117.609231311262,118.605919712205,119.602608113147,120.494711874442),
 .UNSPECIFIED.);
#419=B_SPLINE_CURVE_WITH_KNOTS('',3,(#31217,#31218,#31219,#31220,#31221,
#31222,#31223,#31224,#31225,#31226,#31227,#31228,#31229,#31230,#31231,#31232,
#31233,#31234,#31235,#31236,#31237,#31238,#31239,#31240,#31241),
 .UNSPECIFIED.,.F.,.F.,(4,3,3,3,3,3,3,3,4),(-129.75624789243,-129.569492122576,
-128.572803721634,-127.576115320691,-126.579426919748,-125.582738518805,
-124.586050117862,-123.589361716919,-123.473062585251),.UNSPECIFIED.);
#420=B_SPLINE_CURVE_WITH_KNOTS('',3,(#31242,#31243,#31244,#31245,#31246,
#31247,#31248,#31249,#31250,#31251,#31252,#31253,#31254,#31255,#31256,#31257,
#31258,#31259,#31260,#31261,#31262,#31263,#31264,#31265,#31266),
 .UNSPECIFIED.,.F.,.F.,(4,3,3,3,3,3,3,3,4),(120.494711874442,120.59929651409,
121.595984915033,122.592673315976,123.589361716919,124.586050117862,125.582738518805,
126.579426919748,126.777897181621),.UNSPECIFIED.);
#421=B_SPLINE_CURVE_WITH_KNOTS('',3,(#31271,#31272,#31273,#31274,#31275,
#31276,#31277,#31278,#31279,#31280,#31281,#31282,#31283,#31284,#31285,#31286,
#31287,#31288,#31289,#31290,#31291,#31292),.UNSPECIFIED.,.F.,.F.,(4,3,3,
3,3,3,3,4),(-136.03943319961,-135.549622528234,-134.552934127291,-133.556245726348,
-132.559557325405,-131.562868924462,-130.566180523519,-129.75624789243),
 .UNSPECIFIED.);
#422=B_SPLINE_CURVE_WITH_KNOTS('',3,(#31293,#31294,#31295,#31296,#31297,
#31298,#31299,#31300,#31301,#31302,#31303,#31304,#31305,#31306,#31307,#31308,
#31309,#31310,#31311,#31312,#31313,#31314),.UNSPECIFIED.,.F.,.F.,(4,3,3,
3,3,3,3,4),(126.777897181621,127.576115320691,128.572803721634,129.569492122576,
130.566180523519,131.562868924462,132.559557325405,133.061082488801),
 .UNSPECIFIED.);
#423=B_SPLINE_CURVE_WITH_KNOTS('',3,(#31319,#31320,#31321,#31322,#31323,
#31324,#31325,#31326,#31327,#31328,#31329,#31330,#31331,#31332,#31333,#31334,
#31335,#31336,#31337,#31338,#31339,#31340),.UNSPECIFIED.,.F.,.F.,(4,3,3,
3,3,3,3,4),(-142.322618506789,-141.529752933891,-140.533064532948,-139.536376132005,
-138.539687731062,-137.54299933012,-136.546310929177,-136.03943319961),
 .UNSPECIFIED.);
#424=B_SPLINE_CURVE_WITH_KNOTS('',3,(#31341,#31342,#31343,#31344,#31345,
#31346,#31347,#31348,#31349,#31350,#31351,#31352,#31353,#31354,#31355,#31356,
#31357,#31358,#31359,#31360,#31361,#31362),.UNSPECIFIED.,.F.,.F.,(4,3,3,
3,3,3,3,4),(133.061082488801,133.556245726348,134.552934127291,135.549622528234,
136.546310929177,137.54299933012,138.539687731063,139.344267795981),
 .UNSPECIFIED.);
#425=B_SPLINE_CURVE_WITH_KNOTS('',3,(#31367,#31368,#31369,#31370,#31371,
#31372,#31373,#31374,#31375,#31376,#31377,#31378,#31379,#31380,#31381,#31382,
#31383,#31384,#31385,#31386,#31387,#31388,#31389,#31390,#31391),
 .UNSPECIFIED.,.F.,.F.,(4,3,3,3,3,3,3,3,4),(-148.605803813969,-148.506571740491,
-147.509883339549,-146.513194938606,-145.516506537663,-144.51981813672,
-143.523129735777,-142.526441334834,-142.322618506789),.UNSPECIFIED.);
#426=B_SPLINE_CURVE_WITH_KNOTS('',3,(#31392,#31393,#31394,#31395,#31396,
#31397,#31398,#31399,#31400,#31401,#31402,#31403,#31404,#31405,#31406,#31407,
#31408,#31409,#31410,#31411,#31412,#31413,#31414,#31415,#31416),
 .UNSPECIFIED.,.F.,.F.,(4,3,3,3,3,3,3,3,4),(139.344267795981,139.536376132005,
140.533064532948,141.529752933891,142.526441334834,143.523129735777,144.51981813672,
145.516506537663,145.62745310316),.UNSPECIFIED.);
#427=B_SPLINE_CURVE_WITH_KNOTS('',3,(#31421,#31422,#31423,#31424,#31425,
#31426,#31427,#31428,#31429,#31430,#31431,#31432,#31433,#31434,#31435,#31436,
#31437,#31438,#31439,#31440,#31441,#31442),.UNSPECIFIED.,.F.,.F.,(4,3,3,
3,3,3,3,4),(-154.888989121148,-154.486702146149,-153.490013745206,-152.493325344263,
-151.49663694332,-150.499948542377,-149.503260141434,-148.605803813969),
 .UNSPECIFIED.);
#428=B_SPLINE_CURVE_WITH_KNOTS('',3,(#31443,#31444,#31445,#31446,#31447,
#31448,#31449,#31450,#31451,#31452,#31453,#31454,#31455,#31456,#31457,#31458,
#31459,#31460,#31461,#31462,#31463,#31464),.UNSPECIFIED.,.F.,.F.,(4,3,3,
3,3,3,3,4),(145.62745310316,146.513194938606,147.509883339549,148.506571740491,
149.503260141434,150.499948542377,151.49663694332,151.91063841034),
 .UNSPECIFIED.);
#429=B_SPLINE_CURVE_WITH_KNOTS('',3,(#31469,#31470,#31471,#31472,#31473,
#31474,#31475,#31476,#31477,#31478,#31479,#31480,#31481,#31482,#31483,#31484,
#31485,#31486,#31487,#31488,#31489,#31490),.UNSPECIFIED.,.F.,.F.,(4,3,3,
3,3,3,3,4),(-161.172174428328,-160.466832551806,-159.470144150863,-158.47345574992,
-157.476767348977,-156.480078948035,-155.483390547092,-154.888989121148),
 .UNSPECIFIED.);
#430=B_SPLINE_CURVE_WITH_KNOTS('',3,(#31491,#31492,#31493,#31494,#31495,
#31496,#31497,#31498,#31499,#31500,#31501,#31502,#31503,#31504,#31505,#31506,
#31507,#31508,#31509,#31510,#31511,#31512),.UNSPECIFIED.,.F.,.F.,(4,3,3,
3,3,3,3,4),(151.91063841034,152.493325344263,153.490013745206,154.486702146149,
155.483390547092,156.480078948035,157.476767348978,158.193823717519),
 .UNSPECIFIED.);
#431=B_SPLINE_CURVE_WITH_KNOTS('',3,(#31517,#31518,#31519,#31520,#31521,
#31522,#31523,#31524,#31525,#31526,#31527,#31528,#31529,#31530,#31531,#31532,
#31533,#31534,#31535,#31536,#31537,#31538,#31539,#31540,#31541),
 .UNSPECIFIED.,.F.,.F.,(4,3,3,3,3,3,3,3,4),(-167.455359735507,-167.443651358406,
-166.446962957464,-165.450274556521,-164.453586155578,-163.456897754635,
-162.460209353692,-161.463520952749,-161.172174428328),.UNSPECIFIED.);
#432=B_SPLINE_CURVE_WITH_KNOTS('',3,(#31542,#31543,#31544,#31545,#31546,
#31547,#31548,#31549,#31550,#31551,#31552,#31553,#31554,#31555,#31556,#31557,
#31558,#31559,#31560,#31561,#31562,#31563,#31564,#31565,#31566),
 .UNSPECIFIED.,.F.,.F.,(4,3,3,3,3,3,3,3,4),(158.193823717519,158.47345574992,
159.470144150863,160.466832551806,161.463520952749,162.460209353692,163.456897754635,
164.453586155578,164.477009024699),.UNSPECIFIED.);
#433=B_SPLINE_CURVE_WITH_KNOTS('',3,(#31571,#31572,#31573,#31574,#31575,
#31576,#31577,#31578,#31579,#31580,#31581,#31582,#31583,#31584,#31585,#31586,
#31587,#31588,#31589,#31590,#31591,#31592),.UNSPECIFIED.,.F.,.F.,(4,3,3,
3,3,3,3,4),(-173.738545042687,-173.423781764064,-172.427093363121,-171.430404962178,
-170.433716561235,-169.437028160292,-168.440339759349,-167.455359735507),
 .UNSPECIFIED.);
#434=B_SPLINE_CURVE_WITH_KNOTS('',3,(#31593,#31594,#31595,#31596,#31597,
#31598,#31599,#31600,#31601,#31602,#31603,#31604,#31605,#31606,#31607,#31608,
#31609,#31610,#31611,#31612,#31613,#31614),.UNSPECIFIED.,.F.,.F.,(4,3,3,
3,3,3,3,4),(164.477009024699,165.450274556521,166.446962957464,167.443651358406,
168.440339759349,169.437028160292,170.433716561235,170.760194331878),
 .UNSPECIFIED.);
#435=B_SPLINE_CURVE_WITH_KNOTS('',3,(#31620,#31621,#31622,#31623,#31624,
#31625),.UNSPECIFIED.,.F.,.F.,(4,1,1,4),(185.353966561798,186.035891684118,
187.03258008506,187.957505154611),.UNSPECIFIED.);
#436=B_SPLINE_CURVE_WITH_KNOTS('',3,(#31628,#31629,#31630,#31631,#31632),
 .UNSPECIFIED.,.F.,.F.,(4,1,4),(185.353966561798,185.721122290575,186.717810691518),
 .UNSPECIFIED.);
#437=B_SPLINE_CURVE_WITH_KNOTS('',3,(#31637,#31638,#31639,#31640,#31641,
#31642,#31643,#31644,#31645,#31646),.UNSPECIFIED.,.F.,.F.,(4,1,1,1,1,1,
1,4),(179.070781254618,180.05576127846,181.052449679403,182.049138080346,
183.045826481289,184.042514882232,185.039203283175,185.353966561798),
 .UNSPECIFIED.);
#438=B_SPLINE_CURVE_WITH_KNOTS('',3,(#31647,#31648,#31649,#31650,#31651,
#31652,#31653,#31654,#31655,#31656),.UNSPECIFIED.,.F.,.F.,(4,1,1,1,1,1,
1,4),(179.070781254618,179.740991884918,180.737680285861,181.734368686804,
182.731057087747,183.72774548869,184.724433889632,185.353966561798),
 .UNSPECIFIED.);
#439=B_SPLINE_CURVE_WITH_KNOTS('',3,(#31661,#31662,#31663,#31664,#31665,
#31666,#31667,#31668,#31669,#31670,#31671),.UNSPECIFIED.,.F.,.F.,(4,1,1,
1,1,1,1,1,4),(172.787595947439,173.07894247186,174.075630872803,175.072319273746,
176.069007674689,177.065696075631,178.062384476574,179.059072877517,179.070781254618),
 .UNSPECIFIED.);
#440=B_SPLINE_CURVE_WITH_KNOTS('',3,(#31672,#31673,#31674,#31675,#31676,
#31677,#31678,#31679,#31680,#31681),.UNSPECIFIED.,.F.,.F.,(4,1,1,1,1,1,
1,4),(172.787595947439,173.760861479261,174.757549880203,175.754238281146,
176.750926682089,177.747615083032,178.744303483975,179.070781254618),
 .UNSPECIFIED.);
#441=B_SPLINE_CURVE_WITH_KNOTS('',3,(#31686,#31687,#31688,#31689,#31690,
#31691,#31692,#31693,#31694,#31695),.UNSPECIFIED.,.F.,.F.,(4,1,1,1,1,1,
1,4),(166.504410640259,167.098812066202,168.095500467145,169.092188868088,
170.088877269031,171.085565669974,172.082254070917,172.787595947439),
 .UNSPECIFIED.);
#442=B_SPLINE_CURVE_WITH_KNOTS('',3,(#31696,#31697,#31698,#31699,#31700,
#31701,#31702,#31703,#31704,#31705,#31706),.UNSPECIFIED.,.F.,.F.,(4,1,1,
1,1,1,1,1,4),(166.504410640259,166.78404267266,167.780731073603,168.777419474546,
169.774107875489,170.770796276432,171.767484677375,172.764173078318,172.787595947439),
 .UNSPECIFIED.);
#443=B_SPLINE_CURVE_WITH_KNOTS('',3,(#31711,#31712,#31713,#31714,#31715,
#31716,#31717,#31718,#31719,#31720),.UNSPECIFIED.,.F.,.F.,(4,1,1,1,1,1,
1,4),(160.22122533308,161.118681660545,162.115370061488,163.112058462431,
164.108746863374,165.105435264317,166.10212366526,166.504410640259),
 .UNSPECIFIED.);
#444=B_SPLINE_CURVE_WITH_KNOTS('',3,(#31721,#31722,#31723,#31724,#31725,
#31726,#31727,#31728,#31729,#31730),.UNSPECIFIED.,.F.,.F.,(4,1,1,1,1,1,
1,4),(160.22122533308,160.803912267003,161.800600667946,162.797289068889,
163.793977469832,164.790665870775,165.787354271717,166.504410640259),
 .UNSPECIFIED.);
#445=B_SPLINE_CURVE_WITH_KNOTS('',3,(#31735,#31736,#31737,#31738,#31739,
#31740,#31741,#31742,#31743,#31744,#31745),.UNSPECIFIED.,.F.,.F.,(4,1,1,
1,1,1,1,1,4),(153.9380400259,154.141862853945,155.138551254888,156.135239655831,
157.131928056774,158.128616457716,159.125304858659,160.121993259602,160.22122533308),
 .UNSPECIFIED.);
#446=B_SPLINE_CURVE_WITH_KNOTS('',3,(#31746,#31747,#31748,#31749,#31750,
#31751,#31752,#31753,#31754,#31755),.UNSPECIFIED.,.F.,.F.,(4,1,1,1,1,1,
1,4),(153.9380400259,154.823781861346,155.820470262288,156.817158663231,
157.813847064174,158.810535465117,159.80722386606,160.22122533308),
 .UNSPECIFIED.);
#447=B_SPLINE_CURVE_WITH_KNOTS('',3,(#31760,#31761,#31762,#31763,#31764,
#31765,#31766,#31767,#31768,#31769),.UNSPECIFIED.,.F.,.F.,(4,1,1,1,1,1,
1,4),(147.65485471872,148.161732448287,149.15842084923,150.155109250173,
151.151797651116,152.148486052059,153.145174453002,153.9380400259),
 .UNSPECIFIED.);
#448=B_SPLINE_CURVE_WITH_KNOTS('',3,(#31770,#31771,#31772,#31773,#31774,
#31775,#31776,#31777,#31778,#31779,#31780),.UNSPECIFIED.,.F.,.F.,(4,1,1,
1,1,1,1,1,4),(147.65485471872,147.846963054745,148.843651455688,149.840339856631,
150.837028257574,151.833716658517,152.83040505946,153.827093460403,153.9380400259),
 .UNSPECIFIED.);
#449=B_SPLINE_CURVE_WITH_KNOTS('',3,(#31785,#31786,#31787,#31788,#31789,
#31790,#31791,#31792,#31793,#31794),.UNSPECIFIED.,.F.,.F.,(4,1,1,1,1,1,
1,4),(141.371669411541,142.18160204263,143.178290443573,144.174978844516,
145.171667245459,146.168355646402,147.165044047345,147.65485471872),
 .UNSPECIFIED.);
#450=B_SPLINE_CURVE_WITH_KNOTS('',3,(#31795,#31796,#31797,#31798,#31799,
#31800,#31801,#31802,#31803,#31804),.UNSPECIFIED.,.F.,.F.,(4,1,1,1,1,1,
1,4),(141.371669411541,141.866832649088,142.863521050031,143.860209450974,
144.856897851917,145.85358625286,146.850274653802,147.65485471872),
 .UNSPECIFIED.);
#451=B_SPLINE_CURVE_WITH_KNOTS('',3,(#31809,#31810,#31811,#31812,#31813,
#31814,#31815,#31816,#31817,#31818,#31819),.UNSPECIFIED.,.F.,.F.,(4,1,1,
1,1,1,1,1,4),(135.088484104361,135.20478323603,136.201471636973,137.198160037916,
138.194848438859,139.191536839801,140.188225240744,141.184913641687,141.371669411541),
 .UNSPECIFIED.);
#452=B_SPLINE_CURVE_WITH_KNOTS('',3,(#31820,#31821,#31822,#31823,#31824,
#31825,#31826,#31827,#31828,#31829),.UNSPECIFIED.,.F.,.F.,(4,1,1,1,1,1,
1,4),(135.088484104361,135.886702243431,136.883390644373,137.880079045316,
138.876767446259,139.873455847202,140.870144248145,141.371669411541),
 .UNSPECIFIED.);
#453=B_SPLINE_CURVE_WITH_KNOTS('',3,(#31834,#31835,#31836,#31837,#31838,
#31839,#31840,#31841,#31842,#31843),.UNSPECIFIED.,.F.,.F.,(4,1,1,1,1,1,
1,4),(128.805298797182,129.224652830372,130.221341231315,131.218029632258,
132.214718033201,133.211406434144,134.208094835087,135.088484104361),
 .UNSPECIFIED.);
#454=B_SPLINE_CURVE_WITH_KNOTS('',3,(#31844,#31845,#31846,#31847,#31848,
#31849,#31850,#31851,#31852,#31853,#31854),.UNSPECIFIED.,.F.,.F.,(4,1,1,
1,1,1,1,1,4),(128.805298797182,128.90988343683,129.906571837773,130.903260238716,
131.899948639659,132.896637040602,133.893325441545,134.890013842488,135.088484104361),
 .UNSPECIFIED.);
#455=B_SPLINE_CURVE_WITH_KNOTS('',3,(#31859,#31860,#31861,#31862,#31863,
#31864,#31865,#31866,#31867,#31868),.UNSPECIFIED.,.F.,.F.,(4,1,1,1,1,1,
1,4),(122.522113490002,123.244522424715,124.241210825658,125.237899226601,
126.234587627544,127.231276028487,128.22796442943,128.805298797182),
 .UNSPECIFIED.);
#456=B_SPLINE_CURVE_WITH_KNOTS('',3,(#31869,#31870,#31871,#31872,#31873,
#31874,#31875,#31876,#31877,#31878),.UNSPECIFIED.,.F.,.F.,(4,1,1,1,1,1,
1,4),(122.522113490002,122.929753031173,123.926441432116,124.923129833059,
125.919818234002,126.916506634944,127.913195035887,128.805298797182),
 .UNSPECIFIED.);
#457=B_SPLINE_CURVE_WITH_KNOTS('',3,(#31883,#31884,#31885,#31886,#31887,
#31888,#31889,#31890,#31891,#31892,#31893),.UNSPECIFIED.,.F.,.F.,(4,1,1,
1,1,1,1,1,4),(116.238928182822,116.267703618115,117.264392019058,118.261080420001,
119.257768820943,120.254457221886,121.251145622829,122.247834023772,122.522113490002),
 .UNSPECIFIED.);
#458=B_SPLINE_CURVE_WITH_KNOTS('',3,(#31894,#31895,#31896,#31897,#31898,
#31899,#31900,#31901,#31902,#31903),.UNSPECIFIED.,.F.,.F.,(4,1,1,1,1,1,
1,4),(116.238928182823,116.949622625516,117.946311026458,118.942999427401,
119.939687828344,120.936376229287,121.93306463023,122.522113490002),
 .UNSPECIFIED.);
#459=B_SPLINE_CURVE_WITH_KNOTS('',3,(#31908,#31909,#31910,#31911,#31912,
#31913,#31914,#31915,#31916,#31917),.UNSPECIFIED.,.F.,.F.,(4,1,1,1,1,1,
1,4),(109.955742875643,110.287573212457,111.2842616134,112.280950014343,
113.277638415286,114.274326816229,115.271015217172,116.238928182822),
 .UNSPECIFIED.);
#460=B_SPLINE_CURVE_WITH_KNOTS('',3,(#31918,#31919,#31920,#31921,#31922,
#31923,#31924,#31925,#31926,#31927,#31928),.UNSPECIFIED.,.F.,.F.,(4,1,1,
1,1,1,1,1,4),(109.955742875643,109.972803818915,110.969492219858,111.966180620801,
112.962869021744,113.959557422687,114.95624582363,115.952934224573,116.238928182823),
 .UNSPECIFIED.);
#461=B_SPLINE_CURVE_WITH_KNOTS('',3,(#31933,#31934,#31935,#31936,#31937,
#31938,#31939,#31940,#31941,#31942),.UNSPECIFIED.,.F.,.F.,(4,1,1,1,1,1,
1,4),(103.672557568463,104.3074428068,105.304131207743,106.300819608686,
107.297508009629,108.294196410572,109.290884811515,109.955742875643),
 .UNSPECIFIED.);
#462=B_SPLINE_CURVE_WITH_KNOTS('',3,(#31943,#31944,#31945,#31946,#31947,
#31948,#31949,#31950,#31951,#31952),.UNSPECIFIED.,.F.,.F.,(4,1,1,1,1,1,
1,4),(103.672557568463,103.992673413258,104.989361814201,105.986050215144,
106.982738616087,107.979427017029,108.976115417972,109.955742875643),
 .UNSPECIFIED.);
#463=B_SPLINE_CURVE_WITH_KNOTS('',3,(#31957,#31958,#31959,#31960,#31961,
#31962,#31963,#31964,#31965,#31966),.UNSPECIFIED.,.F.,.F.,(4,1,1,1,1,1,
1,4),(97.3893722612837,98.3273124011427,99.3240008020856,100.320689203028,
101.317377603971,102.314066004914,103.310754405857,103.672557568463),
 .UNSPECIFIED.);
#464=B_SPLINE_CURVE_WITH_KNOTS('',3,(#31967,#31968,#31969,#31970,#31971,
#31972,#31973,#31974,#31975,#31976),.UNSPECIFIED.,.F.,.F.,(4,1,1,1,1,1,
1,4),(97.3893722612837,98.0125430076005,99.0092314085434,100.005919809486,
101.002608210429,101.999296611372,102.995985012315,103.672557568463),
 .UNSPECIFIED.);
#465=B_SPLINE_CURVE_WITH_KNOTS('',3,(#31981,#31982,#31983,#31984,#31985,
#31986,#31987,#31988,#31989,#31990,#31991),.UNSPECIFIED.,.F.,.F.,(4,1,1,
1,1,1,1,1,4),(91.1061869541041,91.3504935945424,92.3471819954853,93.3438703964282,
94.3405587973711,95.337247198314,96.3339355992569,97.3306240001998,97.3893722612837),
 .UNSPECIFIED.);
#466=B_SPLINE_CURVE_WITH_KNOTS('',3,(#31992,#31993,#31994,#31995,#31996,
#31997,#31998,#31999,#32000,#32001),.UNSPECIFIED.,.F.,.F.,(4,1,1,1,1,1,
1,4),(91.1061869541041,92.0324126019432,93.029101002886,94.0257894038289,
95.0224778047718,96.0191662057147,97.0158546066576,97.3893722612837),
 .UNSPECIFIED.);
#467=B_SPLINE_CURVE_WITH_KNOTS('',3,(#32006,#32007,#32008,#32009,#32010,
#32011,#32012,#32013,#32014,#32015),.UNSPECIFIED.,.F.,.F.,(4,1,1,1,1,1,
1,4),(84.8230016469245,85.3703631888851,86.3670515898279,87.3637399907708,
88.3604283917137,89.3571167926566,90.3538051935995,91.1061869541041),
 .UNSPECIFIED.);
#468=B_SPLINE_CURVE_WITH_KNOTS('',3,(#32016,#32017,#32018,#32019,#32020,
#32021,#32022,#32023,#32024,#32025,#32026),.UNSPECIFIED.,.F.,.F.,(4,1,1,
1,1,1,1,1,4),(84.8230016469246,85.0555937953429,86.0522821962858,87.0489705972287,
88.0456589981716,89.0423473991145,90.0390358000574,91.0357242010002,91.1061869541041),
 .UNSPECIFIED.);
#469=B_SPLINE_CURVE_WITH_KNOTS('',3,(#32031,#32032,#32033,#32034,#32035,
#32036,#32037,#32038,#32039,#32040),.UNSPECIFIED.,.F.,.F.,(4,1,1,1,1,1,
1,4),(78.5398163397449,79.3902327832277,80.3869211841706,81.3836095851135,
82.3802979860564,83.3769863869992,84.3736747879422,84.8230016469245),
 .UNSPECIFIED.);
#470=B_SPLINE_CURVE_WITH_KNOTS('',3,(#32041,#32042,#32043,#32044,#32045,
#32046,#32047,#32048,#32049,#32050),.UNSPECIFIED.,.F.,.F.,(4,1,1,1,1,1,
1,4),(78.539816339745,79.0754633896855,80.0721517906284,81.0688401915713,
82.0655285925142,83.0622169934571,84.0589053944,84.8230016469246),
 .UNSPECIFIED.);
#471=B_SPLINE_CURVE_WITH_KNOTS('',3,(#32055,#32056,#32057,#32058,#32059,
#32060,#32061,#32062,#32063,#32064,#32065),.UNSPECIFIED.,.F.,.F.,(4,1,1,
1,1,1,1,1,4),(72.2566310325653,72.4134139766274,73.4101023775703,74.4067907785132,
75.4034791794561,76.400167580399,77.3968559813419,78.3935443822848,78.5398163397449),
 .UNSPECIFIED.);
#472=B_SPLINE_CURVE_WITH_KNOTS('',3,(#32066,#32067,#32068,#32069,#32070,
#32071,#32072,#32073,#32074,#32075),.UNSPECIFIED.,.F.,.F.,(4,1,1,1,1,1,
1,4),(72.2566310325654,73.0953329840281,74.092021384971,75.0887097859139,
76.0853981868568,77.0820865877997,78.0787749887426,78.539816339745),
 .UNSPECIFIED.);
#473=B_SPLINE_CURVE_WITH_KNOTS('',3,(#32080,#32081,#32082,#32083,#32084,
#32085,#32086,#32087,#32088,#32089),.UNSPECIFIED.,.F.,.F.,(4,1,1,1,1,1,
1,4),(65.9734457253857,66.43328357097,67.4299719719129,68.4266603728558,
69.4233487737987,70.4200371747416,71.4167255756845,72.2566310325653),
 .UNSPECIFIED.);
#474=B_SPLINE_CURVE_WITH_KNOTS('',3,(#32090,#32091,#32092,#32093,#32094,
#32095,#32096,#32097,#32098,#32099,#32100),.UNSPECIFIED.,.F.,.F.,(4,1,1,
1,1,1,1,1,4),(65.9734457253858,66.1185141774279,67.1152025783708,68.1118909793137,
69.1085793802565,70.1052677811994,71.1019561821423,72.0986445830852,72.2566310325654),
 .UNSPECIFIED.);
#475=B_SPLINE_CURVE_WITH_KNOTS('',3,(#32105,#32106,#32107,#32108,#32109,
#32110,#32111,#32112,#32113,#32114),.UNSPECIFIED.,.F.,.F.,(4,1,1,1,1,1,
1,4),(59.6902604182062,60.4531531653127,61.4498415662556,62.4465299671985,
63.4432183681413,64.4399067690842,65.4365951700271,65.9734457253857),
 .UNSPECIFIED.);
#476=B_SPLINE_CURVE_WITH_KNOTS('',3,(#32115,#32116,#32117,#32118,#32119,
#32120,#32121,#32122,#32123,#32124),.UNSPECIFIED.,.F.,.F.,(4,1,1,1,1,1,
1,4),(59.6902604182062,60.1383837717705,61.1350721727134,62.1317605736563,
63.1284489745992,64.1251373755421,65.121825776485,65.9734457253858),
 .UNSPECIFIED.);
#477=B_SPLINE_CURVE_WITH_KNOTS('',3,(#32129,#32130,#32131,#32132,#32133,
#32134,#32135,#32136,#32137,#32138,#32139),.UNSPECIFIED.,.F.,.F.,(4,1,1,
1,1,1,1,1,4),(53.4070751110266,53.4763343587124,54.4730227596553,55.4697111605982,
56.4663995615411,57.463087962484,58.4597763634269,59.4564647643698,59.6902604182062),
 .UNSPECIFIED.);
#478=B_SPLINE_CURVE_WITH_KNOTS('',3,(#32140,#32141,#32142,#32143,#32144,
#32145,#32146,#32147,#32148,#32149),.UNSPECIFIED.,.F.,.F.,(4,1,1,1,1,1,
1,4),(53.4070751110266,54.1582533661131,55.154941767056,56.1516301679989,
57.1483185689418,58.1450069698847,59.1416953708276,59.6902604182062),
 .UNSPECIFIED.);
#479=B_SPLINE_CURVE_WITH_KNOTS('',3,(#32154,#32155,#32156,#32157,#32158,
#32159,#32160,#32161,#32162,#32163),.UNSPECIFIED.,.F.,.F.,(4,1,1,1,1,1,
1,4),(47.123889803847,47.496203953055,48.4928923539979,49.4895807549408,
50.4862691558837,51.4829575568266,52.4796459577695,53.4070751110266),
 .UNSPECIFIED.);
#480=B_SPLINE_CURVE_WITH_KNOTS('',3,(#32164,#32165,#32166,#32167,#32168,
#32169,#32170,#32171,#32172,#32173,#32174),.UNSPECIFIED.,.F.,.F.,(4,1,1,
1,1,1,1,1,4),(47.123889803847,47.1814345595128,48.1781229604557,49.1748113613986,
50.1714997623415,51.1681881632844,52.1648765642273,53.1615649651702,53.4070751110266),
 .UNSPECIFIED.);
#481=B_SPLINE_CURVE_WITH_KNOTS('',3,(#32179,#32180,#32181,#32182,#32183,
#32184,#32185,#32186,#32187,#32188),.UNSPECIFIED.,.F.,.F.,(4,1,1,1,1,1,
1,4),(40.8407044966674,41.5160735473976,42.5127619483405,43.5094503492834,
44.5061387502263,45.5028271511692,46.4995155521121,47.123889803847),
 .UNSPECIFIED.);
#482=B_SPLINE_CURVE_WITH_KNOTS('',3,(#32189,#32190,#32191,#32192,#32193,
#32194,#32195,#32196,#32197,#32198),.UNSPECIFIED.,.F.,.F.,(4,1,1,1,1,1,
1,4),(40.8407044966674,41.2013041538555,42.1979925547984,43.1946809557413,
44.1913693566841,45.188057757627,46.18474615857,47.123889803847),
 .UNSPECIFIED.);
#483=B_SPLINE_CURVE_WITH_KNOTS('',3,(#32203,#32204,#32205,#32206,#32207,
#32208,#32209,#32210,#32211,#32212),.UNSPECIFIED.,.F.,.F.,(4,1,1,1,1,1,
1,4),(34.5575191894878,35.5359431417403,36.5326315426832,37.5293199436261,
38.526008344569,39.5226967455119,40.5193851464548,40.8407044966674),
 .UNSPECIFIED.);
#484=B_SPLINE_CURVE_WITH_KNOTS('',3,(#32213,#32214,#32215,#32216,#32217,
#32218,#32219,#32220,#32221,#32222),.UNSPECIFIED.,.F.,.F.,(4,1,1,1,1,1,
1,4),(34.5575191894878,35.2211737481981,36.217862149141,37.2145505500839,
38.2112389510268,39.2079273519697,40.2046157529126,40.8407044966674),
 .UNSPECIFIED.);
#485=B_SPLINE_CURVE_WITH_KNOTS('',3,(#32227,#32228,#32229,#32230,#32231,
#32232,#32233,#32234,#32235,#32236,#32237),.UNSPECIFIED.,.F.,.F.,(4,1,1,
1,1,1,1,1,4),(28.2743338823082,28.55912433514,29.5558127360829,30.5525011370258,
31.5491895379687,32.5458779389116,33.5425663398545,34.5392547407974,34.5575191894878),
 .UNSPECIFIED.);
#486=B_SPLINE_CURVE_WITH_KNOTS('',3,(#32238,#32239,#32240,#32241,#32242,
#32243,#32244,#32245,#32246,#32247),.UNSPECIFIED.,.F.,.F.,(4,1,1,1,1,1,
1,4),(28.2743338823082,29.2410433425407,30.2377317434836,31.2344201444265,
32.2311085453694,33.2277969463123,34.2244853472552,34.5575191894878),
 .UNSPECIFIED.);
#487=B_SPLINE_CURVE_WITH_KNOTS('',3,(#32252,#32253,#32254,#32255,#32256,
#32257,#32258,#32259,#32260,#32261),.UNSPECIFIED.,.F.,.F.,(4,1,1,1,1,1,
1,4),(21.9911485751286,22.5789939294826,23.5756823304255,24.5723707313684,
25.5690591323113,26.5657475332542,27.5624359341971,28.2743338823082),
 .UNSPECIFIED.);
#488=B_SPLINE_CURVE_WITH_KNOTS('',3,(#32262,#32263,#32264,#32265,#32266,
#32267,#32268,#32269,#32270,#32271,#32272),.UNSPECIFIED.,.F.,.F.,(4,1,1,
1,1,1,1,1,4),(21.9911485751286,22.2642245359404,23.2609129368833,24.2576013378262,
25.2542897387691,26.250978139712,27.2476665406549,28.2443549415978,28.2743338823082),
 .UNSPECIFIED.);
#489=B_SPLINE_CURVE_WITH_KNOTS('',3,(#32277,#32278,#32279,#32280,#32281,
#32282,#32283,#32284,#32285,#32286),.UNSPECIFIED.,.F.,.F.,(4,1,1,1,1,1,
1,4),(15.707963267949,16.5988635238253,17.5955519247682,18.592240325711,
19.5889287266539,20.5856171275968,21.5823055285397,21.9911485751286),
 .UNSPECIFIED.);
#490=B_SPLINE_CURVE_WITH_KNOTS('',3,(#32287,#32288,#32289,#32290,#32291,
#32292,#32293,#32294,#32295,#32296),.UNSPECIFIED.,.F.,.F.,(4,1,1,1,1,1,
1,4),(15.7079632679491,16.2840941302831,17.280782531226,18.2774709321689,
19.2741593331118,20.2708477340547,21.2675361349975,21.9911485751286),
 .UNSPECIFIED.);
#491=B_SPLINE_CURVE_WITH_KNOTS('',3,(#33026,#33027,#33028,#33029,#33030,
#33031,#33032,#33033,#33034,#33035,#33036,#33037,#33038,#33039,#33040,#33041,
#33042,#33043,#33044,#33045,#33046,#33047,#33048,#33049,#33050,#33051,#33052,
#33053,#33054,#33055,#33056,#33057,#33058,#33059,#33060,#33061,#33062,#33063,
#33064,#33065,#33066,#33067,#33068,#33069,#33070,#33071,#33072,#33073,#33074,
#33075,#33076,#33077,#33078,#33079,#33080,#33081,#33082,#33083,#33084,#33085,
#33086,#33087,#33088,#33089,#33090,#33091,#33092,#33093,#33094,#33095,#33096,
#33097,#33098,#33099,#33100,#33101,#33102,#33103,#33104,#33105,#33106,#33107,
#33108,#33109,#33110),.UNSPECIFIED.,.F.,.F.,(4,3,3,3,3,3,3,3,3,3,3,3,3,
3,3,3,3,3,3,3,3,3,3,3,3,3,3,3,4),(-0.364629307890677,-0.350633900072411,
-0.329041704670282,-0.318610240360053,-0.314211809209346,-0.309991562440127,
-0.288669495842773,-0.273343246647572,-0.264936046207356,-0.261282518776684,
-0.240547548924119,-0.220305350751337,-0.206743888633794,-0.195908185817342,
-0.191307393253942,-0.171722665567813,-0.166059502281165,-0.145302064496019,
-0.126512361062532,-0.122942915179013,-0.103486325737185,-0.0841149564703082,
-0.0651452351091335,-0.0617524799581062,-0.0585973862637413,-0.0400118512028539,
-0.0217626000928946,-0.00409409640715274,0.),.UNSPECIFIED.);
#492=B_SPLINE_CURVE_WITH_KNOTS('',3,(#33111,#33112,#33113,#33114,#33115,
#33116,#33117,#33118,#33119,#33120,#33121,#33122,#33123,#33124,#33125,#33126,
#33127,#33128,#33129),.UNSPECIFIED.,.F.,.F.,(4,3,3,3,3,3,4),(170.760194331878,
171.430404962178,172.427093363121,173.423781764064,174.420470165007,175.41715856595,
176.3420836355),.UNSPECIFIED.);
#493=B_SPLINE_CURVE_WITH_KNOTS('',3,(#33131,#33132,#33133,#33134,#33135,
#33136,#33137,#33138,#33139,#33140,#33141,#33142,#33143,#33144,#33145,#33146,
#33147,#33148,#33149,#33150,#33151,#33152,#33153,#33154,#33155,#33156,#33157,
#33158,#33159,#33160,#33161,#33162,#33163,#33164,#33165,#33166,#33167,#33168,
#33169,#33170,#33171,#33172,#33173,#33174,#33175,#33176,#33177,#33178,#33179,
#33180,#33181,#33182,#33183,#33184,#33185,#33186,#33187,#33188,#33189,#33190,
#33191,#33192,#33193,#33194,#33195,#33196,#33197,#33198,#33199,#33200,#33201,
#33202,#33203,#33204,#33205,#33206,#33207,#33208,#33209,#33210,#33211,#33212,
#33213,#33214,#33215,#33216,#33217,#33218),.UNSPECIFIED.,.F.,.F.,(4,3,3,
3,3,3,3,3,3,3,3,3,3,3,3,3,3,3,3,3,3,3,3,3,3,3,3,3,3,4),(-0.366397579005836,
-0.355041886299224,-0.337062787725164,-0.326501278567632,-0.321631321273088,
-0.302824937919741,-0.288343590237545,-0.283403867206792,-0.278586063274018,
-0.259172750250793,-0.239354368340686,-0.226259315371058,-0.219843000340891,
-0.21589805551395,-0.212600028401396,-0.192167406827401,-0.186974156462173,
-0.16726465537396,-0.156579741514883,-0.14850118895299,-0.143866273868592,
-0.123388341850169,-0.102479735695224,-0.0814132858967858,-0.0760794007410636,
-0.0722494160080696,-0.050607200648757,-0.0289135329765765,-0.00768187993829445,
0.),.UNSPECIFIED.);
#494=B_SPLINE_CURVE_WITH_KNOTS('',3,(#33219,#33220,#33221,#33222,#33223,
#33224,#33225,#33226,#33227),.UNSPECIFIED.,.F.,.F.,(4,1,1,1,1,1,4),(10.375727056018,
11.3006521255686,12.2973405265115,13.2940289274544,14.2907173283973,15.2874057293402,
15.7079632679491),.UNSPECIFIED.);
#495=B_SPLINE_CURVE_WITH_KNOTS('',3,(#33233,#33234,#33235,#33236,#33237,
#33238,#33239,#33240,#33241,#33242,#33243,#33244,#33245,#33246,#33247,#33248,
#33249,#33250,#33251,#33252,#33253,#33254,#33255,#33256,#33257,#33258,#33259,
#33260,#33261,#33262,#33263,#33264,#33265,#33266,#33267,#33268,#33269,#33270,
#33271,#33272,#33273,#33274,#33275,#33276,#33277,#33278,#33279,#33280,#33281,
#33282,#33283,#33284,#33285,#33286,#33287,#33288,#33289,#33290,#33291,#33292,
#33293,#33294,#33295,#33296,#33297,#33298,#33299,#33300,#33301,#33302,#33303,
#33304,#33305,#33306,#33307,#33308,#33309,#33310,#33311,#33312,#33313,#33314,
#33315,#33316,#33317),.UNSPECIFIED.,.F.,.F.,(4,3,3,3,3,3,3,3,3,3,3,3,3,
3,3,3,3,3,3,3,3,3,3,3,3,3,3,3,4),(-0.364629307890672,-0.350633900072397,
-0.329041704541407,-0.318610239007672,-0.314211805903378,-0.309991556626561,
-0.288669489872321,-0.273343241423426,-0.264936036487681,-0.261282509824091,
-0.240547539435301,-0.22030533709963,-0.206743878395012,-0.19590817040634,
-0.191307393248018,-0.171722661165846,-0.166059502281157,-0.145302064496012,
-0.126512358429279,-0.122942914832795,-0.103486324429666,-0.0841149582984427,
-0.0651452432836519,-0.0617525129582775,-0.0585973930124723,-0.0400118624810509,
-0.0217626179331671,-0.00409412217882526,0.),.UNSPECIFIED.);
#496=B_SPLINE_CURVE_WITH_KNOTS('',3,(#33320,#33321,#33322,#33323,#33324,
#33325,#33326,#33327),.UNSPECIFIED.,.F.,.F.,(4,1,1,1,1,4),(11.6154215191108,
12.6121099200537,13.6087983209966,14.6054867219395,15.6021751228824,15.707963267949),
 .UNSPECIFIED.);
#497=B_SPLINE_CURVE_WITH_KNOTS('',3,(#34057,#34058,#34059,#34060,#34061,
#34062,#34063,#34064,#34065,#34066,#34067,#34068,#34069,#34070,#34071,#34072,
#34073,#34074,#34075,#34076,#34077,#34078,#34079,#34080,#34081,#34082,#34083,
#34084,#34085,#34086,#34087,#34088,#34089,#34090,#34091,#34092,#34093,#34094,
#34095,#34096,#34097,#34098,#34099,#34100,#34101,#34102,#34103,#34104,#34105,
#34106,#34107,#34108,#34109,#34110,#34111,#34112,#34113,#34114,#34115,#34116,
#34117,#34118,#34119,#34120,#34121,#34122,#34123,#34124,#34125,#34126,#34127,
#34128,#34129,#34130,#34131,#34132,#34133,#34134,#34135,#34136,#34137,#34138,
#34139,#34140,#34141,#34142,#34143,#34144),.UNSPECIFIED.,.F.,.F.,(4,3,3,
3,3,3,3,3,3,3,3,3,3,3,3,3,3,3,3,3,3,3,3,3,3,3,3,3,3,4),(-0.366397579005864,
-0.355041886299263,-0.337062782468908,-0.326501268799074,-0.321631319446025,
-0.302824932606277,-0.288343585588267,-0.28340384950488,-0.278586062019024,
-0.25917274616902,-0.23935436447467,-0.226259312471552,-0.219842994646873,
-0.21589802025165,-0.212599984542311,-0.192167363138322,-0.186974156462199,
-0.16726465363277,-0.156579738901073,-0.14850118045862,-0.143866272303297,
-0.123388338113734,-0.102479729738396,-0.0814132797369128,-0.076079391630003,
-0.0722494180511983,-0.050607201191144,-0.0289135346127569,-0.00768188780162423,
0.),.UNSPECIFIED.);
#498=B_SPLINE_CURVE_WITH_KNOTS('',3,(#34145,#34146,#34147,#34148,#34149,
#34150,#34151,#34152,#34153,#34154,#34155,#34156,#34157,#34158,#34159,#34160),
 .UNSPECIFIED.,.F.,.F.,(4,3,3,3,3,4),(-178.407223768778,-177.410535367835,
-176.413846966892,-175.41715856595,-174.420470165007,-173.738545042687),
 .UNSPECIFIED.);
#499=B_SPLINE_CURVE_WITH_KNOTS('',3,(#34169,#34170,#34171,#34172,#34173,
#34174),.UNSPECIFIED.,.F.,.F.,(4,2,4),(1.11299043816547,1.18225571013767,
1.25152098210987),.UNSPECIFIED.);
#500=B_SPLINE_CURVE_WITH_KNOTS('',3,(#34182,#34183,#34184,#34185,#34186,
#34187),.UNSPECIFIED.,.F.,.F.,(4,2,4),(1.11299043816547,1.18225571013767,
1.25152098210987),.UNSPECIFIED.);
#501=B_SPLINE_CURVE_WITH_KNOTS('',3,(#34193,#34194,#34195,#34196,#34197,
#34198),.UNSPECIFIED.,.F.,.F.,(4,2,4),(1.11299043816547,1.18225571013767,
1.25152098210987),.UNSPECIFIED.);
#502=B_SPLINE_CURVE_WITH_KNOTS('',3,(#34204,#34205,#34206,#34207,#34208,
#34209),.UNSPECIFIED.,.F.,.F.,(4,2,4),(1.11299043816547,1.18225571013767,
1.25152098210987),.UNSPECIFIED.);
#503=B_SPLINE_CURVE_WITH_KNOTS('',3,(#34215,#34216,#34217,#34218,#34219,
#34220),.UNSPECIFIED.,.F.,.F.,(4,2,4),(1.11299043816547,1.18225571013767,
1.25152098210987),.UNSPECIFIED.);
#504=B_SPLINE_CURVE_WITH_KNOTS('',3,(#34225,#34226,#34227,#34228,#34229,
#34230),.UNSPECIFIED.,.F.,.F.,(4,2,4),(1.11299043816547,1.18225571013767,
1.25152098210987),.UNSPECIFIED.);
#505=B_SPLINE_CURVE_WITH_KNOTS('',3,(#34463,#34464,#34465,#34466,#34467,
#34468,#34469,#34470,#34471,#34472),.UNSPECIFIED.,.F.,.F.,(4,3,3,4),(-4.09282965349934,
-3.99167035755174,-2.99375276816381,-2.06974660785397),.UNSPECIFIED.);
#506=B_SPLINE_CURVE_WITH_KNOTS('',3,(#34475,#34476,#34477,#34478,#34479,
#34480,#34481),.UNSPECIFIED.,.F.,.F.,(4,3,4),(0.,0.997917589387936,1.11850960794432),
 .UNSPECIFIED.);
#507=B_SPLINE_CURVE_WITH_KNOTS('',3,(#34486,#34487,#34488,#34489,#34490,
#34491,#34492,#34493,#34494,#34495,#34496,#34497,#34498,#34499,#34500,#34501,
#34502,#34503,#34504,#34505,#34506,#34507),.UNSPECIFIED.,.F.,.F.,(4,3,3,
3,3,3,3,4),(-10.3760149606789,-9.97917589387935,-8.98125830449142,-7.98334071510348,
-6.98542312571555,-5.98750553632761,-4.98958794693968,-4.09282965349934),
 .UNSPECIFIED.);
#508=B_SPLINE_CURVE_WITH_KNOTS('',3,(#34508,#34509,#34510,#34511,#34512,
#34513,#34514,#34515,#34516,#34517,#34518,#34519,#34520,#34521,#34522,#34523,
#34524,#34525,#34526,#34527,#34528,#34529),.UNSPECIFIED.,.F.,.F.,(4,3,3,
3,3,3,3,4),(1.11850960794432,1.99583517877587,2.99375276816381,3.99167035755174,
4.98958794693968,5.98750553632761,6.98542312571555,7.40169491512391),
 .UNSPECIFIED.);
#509=B_SPLINE_CURVE_WITH_KNOTS('',3,(#34534,#34535,#34536,#34537,#34538,
#34539,#34540,#34541,#34542,#34543,#34544,#34545,#34546,#34547,#34548,#34549,
#34550,#34551,#34552,#34553,#34554,#34555),.UNSPECIFIED.,.F.,.F.,(4,3,3,
3,3,3,3,4),(-16.6592002678585,-15.966681430207,-14.968763840819,-13.9708462514311,
-12.9729286620432,-11.9750110726552,-10.9770934832673,-10.3760149606789),
 .UNSPECIFIED.);
#510=B_SPLINE_CURVE_WITH_KNOTS('',3,(#34556,#34557,#34558,#34559,#34560,
#34561,#34562,#34563,#34564,#34565,#34566,#34567,#34568,#34569,#34570,#34571,
#34572,#34573,#34574,#34575,#34576,#34577),.UNSPECIFIED.,.F.,.F.,(4,3,3,
3,3,3,3,4),(7.40169491512391,7.98334071510348,8.98125830449142,9.97917589387935,
10.9770934832673,11.9750110726552,12.9729286620432,13.6848802223035),
 .UNSPECIFIED.);
#511=B_SPLINE_CURVE_WITH_KNOTS('',3,(#34582,#34583,#34584,#34585,#34586,
#34587,#34588,#34589,#34590,#34591,#34592,#34593,#34594,#34595,#34596,#34597,
#34598,#34599,#34600,#34601,#34602,#34603),.UNSPECIFIED.,.F.,.F.,(4,3,3,
3,3,3,3,4),(-22.9423855750381,-21.9541869665346,-20.9562693771467,-19.9583517877587,
-18.9604341983708,-17.9625166089828,-16.9645990195949,-16.6592002678585),
 .UNSPECIFIED.);
#512=B_SPLINE_CURVE_WITH_KNOTS('',3,(#34604,#34605,#34606,#34607,#34608,
#34609,#34610,#34611,#34612,#34613,#34614,#34615,#34616,#34617,#34618,#34619,
#34620,#34621,#34622,#34623,#34624,#34625,#34626,#34627,#34628),
 .UNSPECIFIED.,.F.,.F.,(4,3,3,3,3,3,3,3,4),(13.6848802223035,13.9708462514311,
14.968763840819,15.966681430207,16.9645990195949,17.9625166089828,18.9604341983708,
19.9583517877587,19.9680655294831),.UNSPECIFIED.);
#513=B_SPLINE_CURVE_WITH_KNOTS('',3,(#34633,#34634,#34635,#34636,#34637,
#34638,#34639,#34640,#34641,#34642,#34643,#34644,#34645,#34646,#34647,#34648,
#34649,#34650,#34651,#34652,#34653,#34654,#34655,#34656,#34657),
 .UNSPECIFIED.,.F.,.F.,(4,3,3,3,3,3,3,3,4),(-29.2255708822177,-28.9396100922501,
-27.9416925028622,-26.9437749134743,-25.9458573240863,-24.9479397346984,
-23.9500221453105,-22.9521045559225,-22.9423855750381),.UNSPECIFIED.);
#514=B_SPLINE_CURVE_WITH_KNOTS('',3,(#34658,#34659,#34660,#34661,#34662,
#34663,#34664,#34665,#34666,#34667,#34668,#34669,#34670,#34671,#34672,#34673,
#34674,#34675,#34676,#34677,#34678,#34679),.UNSPECIFIED.,.F.,.F.,(4,3,3,
3,3,3,3,4),(19.9680655294831,20.9562693771466,21.9541869665346,22.9521045559225,
23.9500221453104,24.9479397346984,25.9458573240863,26.2512508366627),
 .UNSPECIFIED.);
#515=B_SPLINE_CURVE_WITH_KNOTS('',3,(#34684,#34685,#34686,#34687,#34688,
#34689,#34690,#34691,#34692,#34693,#34694,#34695,#34696,#34697,#34698,#34699,
#34700,#34701,#34702,#34703,#34704,#34705),.UNSPECIFIED.,.F.,.F.,(4,3,3,
3,3,3,3,4),(-35.5087561893973,-34.9271156285777,-33.9291980391898,-32.9312804498019,
-31.9333628604139,-30.935445271026,-29.9375276816381,-29.2255708822177),
 .UNSPECIFIED.);
#516=B_SPLINE_CURVE_WITH_KNOTS('',3,(#34706,#34707,#34708,#34709,#34710,
#34711,#34712,#34713,#34714,#34715,#34716,#34717,#34718,#34719,#34720,#34721,
#34722,#34723,#34724,#34725,#34726,#34727),.UNSPECIFIED.,.F.,.F.,(4,3,3,
3,3,3,3,4),(26.2512508366627,26.9437749134742,27.9416925028622,28.9396100922501,
29.937527681638,30.935445271026,31.9333628604139,32.5344361438423),
 .UNSPECIFIED.);
#517=B_SPLINE_CURVE_WITH_KNOTS('',3,(#34732,#34733,#34734,#34735,#34736,
#34737,#34738,#34739,#34740,#34741,#34742,#34743,#34744,#34745,#34746,#34747,
#34748,#34749,#34750,#34751,#34752,#34753),.UNSPECIFIED.,.F.,.F.,(4,3,3,
3,3,3,3,4),(-41.7919414965769,-40.9146211649053,-39.9167035755174,-38.9187859861295,
-37.9208683967415,-36.9229508073536,-35.9250332179657,-35.5087561893973),
 .UNSPECIFIED.);
#518=B_SPLINE_CURVE_WITH_KNOTS('',3,(#34754,#34755,#34756,#34757,#34758,
#34759,#34760,#34761,#34762,#34763,#34764,#34765,#34766,#34767,#34768,#34769,
#34770,#34771,#34772,#34773,#34774,#34775),.UNSPECIFIED.,.F.,.F.,(4,3,3,
3,3,3,3,4),(32.5344361438423,32.9312804498019,33.9291980391898,34.9271156285777,
35.9250332179657,36.9229508073536,37.9208683967415,38.8176214510219),
 .UNSPECIFIED.);
#519=B_SPLINE_CURVE_WITH_KNOTS('',3,(#34780,#34781,#34782,#34783,#34784,
#34785,#34786,#34787,#34788,#34789,#34790,#34791,#34792,#34793,#34794,#34795,
#34796,#34797,#34798,#34799,#34800,#34801,#34802,#34803,#34804),
 .UNSPECIFIED.,.F.,.F.,(4,3,3,3,3,3,3,3,4),(-48.0751268037565,-47.9000442906209,
-46.902126701233,-45.904209111845,-44.9062915224571,-43.9083739330692,-42.9104563436812,
-41.9125387542933,-41.7919414965769),.UNSPECIFIED.);
#520=B_SPLINE_CURVE_WITH_KNOTS('',3,(#34805,#34806,#34807,#34808,#34809,
#34810,#34811,#34812,#34813,#34814,#34815,#34816,#34817,#34818,#34819,#34820,
#34821,#34822,#34823,#34824,#34825,#34826,#34827,#34828,#34829),
 .UNSPECIFIED.,.F.,.F.,(4,3,3,3,3,3,3,3,4),(38.8176214510219,38.9187859861295,
39.9167035755174,40.9146211649053,41.9125387542933,42.9104563436812,43.9083739330692,
44.9062915224571,45.1008067582014),.UNSPECIFIED.);
#521=B_SPLINE_CURVE_WITH_KNOTS('',3,(#34834,#34835,#34836,#34837,#34838,
#34839,#34840,#34841,#34842,#34843,#34844,#34845,#34846,#34847,#34848,#34849,
#34850,#34851,#34852,#34853,#34854,#34855),.UNSPECIFIED.,.F.,.F.,(4,3,3,
3,3,3,3,4),(-54.358312110936,-53.8875498269485,-52.8896322375606,-51.8917146481726,
-50.8937970587847,-49.8958794693968,-48.8979618800088,-48.0751268037565),
 .UNSPECIFIED.);
#522=B_SPLINE_CURVE_WITH_KNOTS('',3,(#34856,#34857,#34858,#34859,#34860,
#34861,#34862,#34863,#34864,#34865,#34866,#34867,#34868,#34869,#34870,#34871,
#34872,#34873,#34874,#34875,#34876,#34877),.UNSPECIFIED.,.F.,.F.,(4,3,3,
3,3,3,3,4),(45.1008067582014,45.904209111845,46.902126701233,47.9000442906209,
48.8979618800088,49.8958794693968,50.8937970587847,51.383992065381),
 .UNSPECIFIED.);
#523=B_SPLINE_CURVE_WITH_KNOTS('',3,(#34882,#34883,#34884,#34885,#34886,
#34887,#34888,#34889,#34890,#34891,#34892,#34893,#34894,#34895,#34896,#34897,
#34898,#34899,#34900,#34901,#34902,#34903),.UNSPECIFIED.,.F.,.F.,(4,3,3,
3,3,3,3,4),(-60.6414974181156,-59.8750553632761,-58.8771377738882,-57.8792201845003,
-56.8813025951123,-55.8833850057244,-54.8854674163365,-54.358312110936),
 .UNSPECIFIED.);
#524=B_SPLINE_CURVE_WITH_KNOTS('',3,(#34904,#34905,#34906,#34907,#34908,
#34909,#34910,#34911,#34912,#34913,#34914,#34915,#34916,#34917,#34918,#34919,
#34920,#34921,#34922,#34923,#34924,#34925),.UNSPECIFIED.,.F.,.F.,(4,3,3,
3,3,3,3,4),(51.383992065381,51.8917146481726,52.8896322375606,53.8875498269485,
54.8854674163364,55.8833850057244,56.8813025951123,57.6671773725606),
 .UNSPECIFIED.);
#525=B_SPLINE_CURVE_WITH_KNOTS('',3,(#34930,#34931,#34932,#34933,#34934,
#34935,#34936,#34937,#34938,#34939,#34940,#34941,#34942,#34943,#34944,#34945,
#34946,#34947,#34948,#34949,#34950,#34951,#34952,#34953,#34954),
 .UNSPECIFIED.,.F.,.F.,(4,3,3,3,3,3,3,3,4),(-66.9246827252952,-66.8604784889917,
-65.8625608996037,-64.8646433102158,-63.8667257208279,-62.8688081314399,
-61.870890542052,-60.8729729526641,-60.6414974181156),.UNSPECIFIED.);
#526=B_SPLINE_CURVE_WITH_KNOTS('',3,(#34955,#34956,#34957,#34958,#34959,
#34960,#34961,#34962,#34963,#34964,#34965,#34966,#34967,#34968,#34969,#34970,
#34971,#34972,#34973,#34974,#34975,#34976,#34977,#34978,#34979),
 .UNSPECIFIED.,.F.,.F.,(4,3,3,3,3,3,3,3,4),(57.6671773725606,57.8792201845002,
58.8771377738882,59.8750553632761,60.872972952664,61.870890542052,62.8688081314399,
63.8667257208279,63.9503626797402),.UNSPECIFIED.);
#527=B_SPLINE_CURVE_WITH_KNOTS('',3,(#34984,#34985,#34986,#34987,#34988,
#34989,#34990,#34991,#34992,#34993,#34994,#34995,#34996,#34997,#34998,#34999,
#35000,#35001,#35002,#35003,#35004,#35005),.UNSPECIFIED.,.F.,.F.,(4,3,3,
3,3,3,3,4),(-73.2078680324748,-72.8479840253193,-71.8500664359313,-70.8521488465434,
-69.8542312571555,-68.8563136677676,-67.8583960783796,-66.9246827252952),
 .UNSPECIFIED.);
#528=B_SPLINE_CURVE_WITH_KNOTS('',3,(#35006,#35007,#35008,#35009,#35010,
#35011,#35012,#35013,#35014,#35015,#35016,#35017,#35018,#35019,#35020,#35021,
#35022,#35023,#35024,#35025,#35026,#35027),.UNSPECIFIED.,.F.,.F.,(4,3,3,
3,3,3,3,4),(63.9503626797402,64.8646433102158,65.8625608996037,66.8604784889917,
67.8583960783796,68.8563136677676,69.8542312571555,70.2335479869198),
 .UNSPECIFIED.);
#529=B_SPLINE_CURVE_WITH_KNOTS('',3,(#35032,#35033,#35034,#35035,#35036,
#35037,#35038,#35039,#35040,#35041,#35042,#35043,#35044,#35045,#35046,#35047,
#35048,#35049,#35050,#35051,#35052,#35053),.UNSPECIFIED.,.F.,.F.,(4,3,3,
3,3,3,3,4),(-79.4910533396544,-78.8354895616469,-77.837571972259,-76.839654382871,
-75.8417367934831,-74.8438192040951,-73.8459016147072,-73.2078680324748),
 .UNSPECIFIED.);
#530=B_SPLINE_CURVE_WITH_KNOTS('',3,(#35054,#35055,#35056,#35057,#35058,
#35059,#35060,#35061,#35062,#35063,#35064,#35065,#35066,#35067,#35068,#35069,
#35070,#35071,#35072,#35073,#35074,#35075),.UNSPECIFIED.,.F.,.F.,(4,3,3,
3,3,3,3,4),(70.2335479869198,70.8521488465434,71.8500664359314,72.8479840253193,
73.8459016147072,74.8438192040951,75.8417367934831,76.5167332940994),
 .UNSPECIFIED.);
#531=B_SPLINE_CURVE_WITH_KNOTS('',3,(#35080,#35081,#35082,#35083,#35084,
#35085,#35086,#35087,#35088,#35089,#35090,#35091,#35092,#35093,#35094,#35095,
#35096,#35097,#35098,#35099,#35100,#35101),.UNSPECIFIED.,.F.,.F.,(4,3,3,
3,3,3,3,4),(-85.774238646834,-84.8229950979745,-83.8250775085866,-82.8271599191986,
-81.8292423298107,-80.8313247404228,-79.8334071510348,-79.4910533396544),
 .UNSPECIFIED.);
#532=B_SPLINE_CURVE_WITH_KNOTS('',3,(#35102,#35103,#35104,#35105,#35106,
#35107,#35108,#35109,#35110,#35111,#35112,#35113,#35114,#35115,#35116,#35117,
#35118,#35119,#35120,#35121,#35122,#35123),.UNSPECIFIED.,.F.,.F.,(4,3,3,
3,3,3,3,4),(76.5167332940994,76.839654382871,77.8375719722589,78.8354895616469,
79.8334071510348,80.8313247404228,81.8292423298107,82.799918601279),
 .UNSPECIFIED.);
#533=B_SPLINE_CURVE_WITH_KNOTS('',3,(#35128,#35129,#35130,#35131,#35132,
#35133,#35134,#35135,#35136,#35137,#35138,#35139,#35140,#35141,#35142,#35143,
#35144,#35145,#35146,#35147,#35148,#35149,#35150,#35151,#35152),
 .UNSPECIFIED.,.F.,.F.,(4,3,3,3,3,3,3,3,4),(-92.0574239540136,-91.8084182236901,
-90.8105006343021,-89.8125830449142,-88.8146654555263,-87.8167478661383,
-86.8188302767504,-85.8209126873625,-85.774238646834),.UNSPECIFIED.);
#534=B_SPLINE_CURVE_WITH_KNOTS('',3,(#35153,#35154,#35155,#35156,#35157,
#35158,#35159,#35160,#35161,#35162,#35163,#35164,#35165,#35166,#35167,#35168,
#35169,#35170,#35171,#35172,#35173,#35174,#35175,#35176,#35177),
 .UNSPECIFIED.,.F.,.F.,(4,3,3,3,3,3,3,3,4),(82.799918601279,82.8271599191986,
83.8250775085866,84.8229950979745,85.8209126873624,86.8188302767503,87.8167478661383,
88.8146654555262,89.0831039084586),.UNSPECIFIED.);
#535=B_SPLINE_CURVE_WITH_KNOTS('',3,(#35182,#35183,#35184,#35185,#35186,
#35187,#35188,#35189,#35190,#35191,#35192,#35193,#35194,#35195,#35196,#35197,
#35198,#35199,#35200,#35201,#35202,#35203),.UNSPECIFIED.,.F.,.F.,(4,3,3,
3,3,3,3,4),(-98.3406092611932,-97.7959237600177,-96.7980061706297,-95.8000885812418,
-94.8021709918539,-93.8042534024659,-92.806335813078,-92.0574239540136),
 .UNSPECIFIED.);
#536=B_SPLINE_CURVE_WITH_KNOTS('',3,(#35204,#35205,#35206,#35207,#35208,
#35209,#35210,#35211,#35212,#35213,#35214,#35215,#35216,#35217,#35218,#35219,
#35220,#35221,#35222,#35223,#35224,#35225),.UNSPECIFIED.,.F.,.F.,(4,3,3,
3,3,3,3,4),(89.0831039084586,89.8125830449142,90.8105006343021,91.80841822369,
92.806335813078,93.8042534024659,94.8021709918538,95.3662892156382),
 .UNSPECIFIED.);
#537=B_SPLINE_CURVE_WITH_KNOTS('',3,(#35230,#35231,#35232,#35233,#35234,
#35235,#35236,#35237,#35238,#35239,#35240,#35241,#35242,#35243,#35244,#35245,
#35246,#35247,#35248,#35249,#35250,#35251),.UNSPECIFIED.,.F.,.F.,(4,3,3,
3,3,3,3,4),(-104.623794568373,-103.783429296345,-102.785511706957,-101.787594117569,
-100.789676528181,-99.7917589387935,-98.7938413494056,-98.3406092611932),
 .UNSPECIFIED.);
#538=B_SPLINE_CURVE_WITH_KNOTS('',3,(#35252,#35253,#35254,#35255,#35256,
#35257,#35258,#35259,#35260,#35261,#35262,#35263,#35264,#35265,#35266,#35267,
#35268,#35269,#35270,#35271,#35272,#35273),.UNSPECIFIED.,.F.,.F.,(4,3,3,
3,3,3,3,4),(95.3662892156382,95.8000885812418,96.7980061706297,97.7959237600176,
98.7938413494056,99.7917589387935,100.789676528181,101.649474522818),
 .UNSPECIFIED.);
#539=B_SPLINE_CURVE_WITH_KNOTS('',3,(#35280,#35281,#35282,#35283,#35284,
#35285,#35286,#35287,#35288,#35289,#35290,#35291,#35292,#35293,#35294,#35295,
#35296,#35297,#35298,#35299,#35300,#35301),.UNSPECIFIED.,.F.,.F.,(4,3,3,
3,3,3,3,4),(-110.768852422061,-109.770934832673,-108.773017243285,-107.775099653897,
-106.777182064509,-105.779264475121,-104.781346885733,-104.623794568373),
 .UNSPECIFIED.);
#540=B_SPLINE_CURVE_WITH_KNOTS('',3,(#35302,#35303,#35304,#35305,#35306,
#35307,#35308,#35309,#35310,#35311,#35312,#35313,#35314,#35315,#35316,#35317,
#35318,#35319,#35320,#35321,#35322,#35323,#35324,#35325,#35326),
 .UNSPECIFIED.,.F.,.F.,(4,3,3,3,3,3,3,3,4),(101.649474522818,101.787594117569,
102.785511706957,103.783429296345,104.781346885733,105.779264475121,106.777182064509,
107.775099653897,107.932659829997),.UNSPECIFIED.);
#541=B_SPLINE_CURVE_WITH_KNOTS('',3,(#35332,#35333,#35334,#35335,#35336,
#35337,#35338,#35339),.UNSPECIFIED.,.F.,.F.,(4,1,1,1,1,4),(116.238928182822,
116.396480500183,117.394398089571,118.392315678959,119.390233268347,120.314239428656),
 .UNSPECIFIED.);
#542=B_SPLINE_CURVE_WITH_KNOTS('',3,(#35342,#35343,#35344,#35345,#35346,
#35347),.UNSPECIFIED.,.F.,.F.,(4,1,1,4),(116.238928182822,117.07928559611,
118.077203185498,119.075120774886),.UNSPECIFIED.);
#543=B_SPLINE_CURVE_WITH_KNOTS('',3,(#35352,#35353,#35354,#35355,#35356,
#35357,#35358,#35359,#35360,#35361),.UNSPECIFIED.,.F.,.F.,(4,1,1,1,1,1,
1,4),(109.955742875643,110.408974963855,111.406892553243,112.404810142631,
113.402727732019,114.400645321407,115.398562910795,116.238928182822),
 .UNSPECIFIED.);
#544=B_SPLINE_CURVE_WITH_KNOTS('',3,(#35362,#35363,#35364,#35365,#35366,
#35367,#35368,#35369,#35370,#35371,#35372),.UNSPECIFIED.,.F.,.F.,(4,1,1,
1,1,1,1,1,4),(109.955742875643,110.093862470394,111.091780059782,112.08969764917,
113.087615238558,114.085532827946,115.083450417334,116.081368006722,116.238928182822),
 .UNSPECIFIED.);
#545=B_SPLINE_CURVE_WITH_KNOTS('',3,(#35377,#35378,#35379,#35380,#35381,
#35382,#35383,#35384,#35385,#35386),.UNSPECIFIED.,.F.,.F.,(4,1,1,1,1,1,
1,4),(103.672557568463,104.421469427528,105.419387016915,106.417304606303,
107.415222195691,108.413139785079,109.411057374467,109.955742875643),
 .UNSPECIFIED.);
#546=B_SPLINE_CURVE_WITH_KNOTS('',3,(#35387,#35388,#35389,#35390,#35391,
#35392,#35393,#35394,#35395,#35396),.UNSPECIFIED.,.F.,.F.,(4,1,1,1,1,1,
1,4),(103.672557568463,104.106356934067,105.104274523455,106.102192112842,
107.10010970223,108.098027291618,109.095944881006,109.955742875643),
 .UNSPECIFIED.);
#547=B_SPLINE_CURVE_WITH_KNOTS('',3,(#35401,#35402,#35403,#35404,#35405,
#35406,#35407,#35408,#35409,#35410,#35411),.UNSPECIFIED.,.F.,.F.,(4,1,1,
1,1,1,1,1,4),(97.3893722612836,97.436046301812,98.4339638911999,99.4318814805878,
100.429799069976,101.427716659364,102.425634248752,103.42355183814,103.672557568463),
 .UNSPECIFIED.);
#548=B_SPLINE_CURVE_WITH_KNOTS('',3,(#35412,#35413,#35414,#35415,#35416,
#35417,#35418,#35419,#35420,#35421),.UNSPECIFIED.,.F.,.F.,(4,1,1,1,1,1,
1,4),(97.3893722612836,98.118851397739,99.1167689871269,100.114686576515,
101.112604165903,102.110521755291,103.108439344679,103.672557568463),
 .UNSPECIFIED.);
#549=B_SPLINE_CURVE_WITH_KNOTS('',3,(#35426,#35427,#35428,#35429,#35430,
#35431,#35432,#35433,#35434,#35435),.UNSPECIFIED.,.F.,.F.,(4,1,1,1,1,1,
1,4),(91.106186954104,91.4485407654844,92.4464583548723,93.4443759442602,
94.4422935336482,95.4402111230361,96.438128712424,97.3893722612836),
 .UNSPECIFIED.);
#550=B_SPLINE_CURVE_WITH_KNOTS('',3,(#35436,#35437,#35438,#35439,#35440,
#35441,#35442,#35443,#35444,#35445,#35446),.UNSPECIFIED.,.F.,.F.,(4,1,1,
1,1,1,1,1,4),(91.106186954104,91.1334282720235,92.1313458614114,93.1292634507993,
94.1271810401873,95.1250986295752,96.1230162189631,97.1209338083511,97.3893722612836),
 .UNSPECIFIED.);
#551=B_SPLINE_CURVE_WITH_KNOTS('',3,(#35451,#35452,#35453,#35454,#35455,
#35456,#35457,#35458,#35459,#35460),.UNSPECIFIED.,.F.,.F.,(4,1,1,1,1,1,
1,4),(84.8230016469244,85.4610352291567,86.4589528185447,87.4568704079326,
88.4547879973206,89.4527055867085,90.4506231760964,91.106186954104),
 .UNSPECIFIED.);
#552=B_SPLINE_CURVE_WITH_KNOTS('',3,(#35461,#35462,#35463,#35464,#35465,
#35466,#35467,#35468,#35469,#35470),.UNSPECIFIED.,.F.,.F.,(4,1,1,1,1,1,
1,4),(84.8230016469244,85.1459227356958,86.1438403250838,87.1417579144717,
88.1396755038596,89.1375930932476,90.1355106826355,91.106186954104),
 .UNSPECIFIED.);
#553=B_SPLINE_CURVE_WITH_KNOTS('',3,(#35475,#35476,#35477,#35478,#35479,
#35480,#35481,#35482,#35483,#35484),.UNSPECIFIED.,.F.,.F.,(4,1,1,1,1,1,
1,4),(78.5398163397448,79.4735296928291,80.4714472822171,81.469364871605,
82.4672824609929,83.4652000503809,84.4631176397688,84.8230016469244),
 .UNSPECIFIED.);
#554=B_SPLINE_CURVE_WITH_KNOTS('',3,(#35485,#35486,#35487,#35488,#35489,
#35490,#35491,#35492,#35493,#35494),.UNSPECIFIED.,.F.,.F.,(4,1,1,1,1,1,
1,4),(78.5398163397448,79.1584171993682,80.1563347887562,81.1542523781441,
82.152169967532,83.15008755692,84.1480051463079,84.8230016469244),
 .UNSPECIFIED.);
#555=B_SPLINE_CURVE_WITH_KNOTS('',3,(#35499,#35500,#35501,#35502,#35503,
#35504,#35505,#35506,#35507,#35508,#35509),.UNSPECIFIED.,.F.,.F.,(4,1,1,
1,1,1,1,1,4),(72.2566310325652,72.4881065671136,73.4860241565015,74.4839417458895,
75.4818593352774,76.4797769246653,77.4776945140533,78.4756121034412,78.5398163397448),
 .UNSPECIFIED.);
#556=B_SPLINE_CURVE_WITH_KNOTS('',3,(#35510,#35511,#35512,#35513,#35514,
#35515,#35516,#35517,#35518,#35519),.UNSPECIFIED.,.F.,.F.,(4,1,1,1,1,1,
1,4),(72.2566310325652,73.1709116630406,74.1688292524286,75.1667468418165,
76.1646644312044,77.1625820205924,78.1604996099803,78.5398163397448),
 .UNSPECIFIED.);
#557=B_SPLINE_CURVE_WITH_KNOTS('',3,(#35524,#35525,#35526,#35527,#35528,
#35529,#35530,#35531,#35532,#35533),.UNSPECIFIED.,.F.,.F.,(4,1,1,1,1,1,
1,4),(65.9734457253856,66.500601030786,67.4985186201739,68.4964362095618,
69.4943537989498,70.4922713883377,71.4901889777257,72.2566310325652),
 .UNSPECIFIED.);
#558=B_SPLINE_CURVE_WITH_KNOTS('',3,(#35534,#35535,#35536,#35537,#35538,
#35539,#35540,#35541,#35542,#35543,#35544),.UNSPECIFIED.,.F.,.F.,(4,1,1,
1,1,1,1,1,4),(65.9734457253856,66.1854885373251,67.183406126713,68.1813237161009,
69.1792413054889,70.1771588948768,71.1750764842647,72.1729940736527,72.2566310325652),
 .UNSPECIFIED.);
#559=B_SPLINE_CURVE_WITH_KNOTS('',3,(#35549,#35550,#35551,#35552,#35553,
#35554,#35555,#35556,#35557,#35558),.UNSPECIFIED.,.F.,.F.,(4,1,1,1,1,1,
1,4),(59.690260418206,60.5130954944584,61.5110130838463,62.5089306732342,
63.5068482626222,64.5047658520101,65.502683441398,65.9734457253856),
 .UNSPECIFIED.);
#560=B_SPLINE_CURVE_WITH_KNOTS('',3,(#35559,#35560,#35561,#35562,#35563,
#35564,#35565,#35566,#35567,#35568),.UNSPECIFIED.,.F.,.F.,(4,1,1,1,1,1,
1,4),(59.690260418206,60.1979830009975,61.1959005903854,62.1938181797733,
63.1917357691613,64.1896533585492,65.1875709479371,65.9734457253856),
 .UNSPECIFIED.);
#561=B_SPLINE_CURVE_WITH_KNOTS('',3,(#35573,#35574,#35575,#35576,#35577,
#35578,#35579,#35580,#35581,#35582,#35583),.UNSPECIFIED.,.F.,.F.,(4,1,1,
1,1,1,1,1,4),(53.4070751110264,53.5276723687428,54.5255899581308,55.5235075475187,
56.5214251369066,57.5193427262946,58.5172603156825,59.5151779050704,59.690260418206),
 .UNSPECIFIED.);
#562=B_SPLINE_CURVE_WITH_KNOTS('',3,(#35584,#35585,#35586,#35587,#35588,
#35589,#35590,#35591,#35592,#35593),.UNSPECIFIED.,.F.,.F.,(4,1,1,1,1,1,
1,4),(53.4070751110264,54.2104774646699,55.2083950540578,56.2063126434457,
57.2042302328337,58.2021478222216,59.2000654116095,59.690260418206),
 .UNSPECIFIED.);
#563=B_SPLINE_CURVE_WITH_KNOTS('',3,(#35598,#35599,#35600,#35601,#35602,
#35603,#35604,#35605,#35606,#35607),.UNSPECIFIED.,.F.,.F.,(4,1,1,1,1,1,
1,4),(47.1238898038469,47.5401668324152,48.5380844218031,49.5360020111911,
50.533919600579,51.5318371899669,52.5297547793549,53.4070751110264),
 .UNSPECIFIED.);
#564=B_SPLINE_CURVE_WITH_KNOTS('',3,(#35608,#35609,#35610,#35611,#35612,
#35613,#35614,#35615,#35616,#35617,#35618),.UNSPECIFIED.,.F.,.F.,(4,1,1,
1,1,1,1,1,4),(47.1238898038468,47.2250543389543,48.2229719283422,49.2208895177302,
50.2188071071181,51.216724696506,52.214642285894,53.2125598752819,53.4070751110264),
 .UNSPECIFIED.);
#565=B_SPLINE_CURVE_WITH_KNOTS('',3,(#35623,#35624,#35625,#35626,#35627,
#35628,#35629,#35630,#35631,#35632),.UNSPECIFIED.,.F.,.F.,(4,1,1,1,1,1,
1,4),(40.8407044966672,41.5526612960876,42.5505788854755,43.5484964748635,
44.5464140642514,45.5443316536393,46.5422492430273,47.1238898038469),
 .UNSPECIFIED.);
#566=B_SPLINE_CURVE_WITH_KNOTS('',3,(#35633,#35634,#35635,#35636,#35637,
#35638,#35639,#35640,#35641,#35642),.UNSPECIFIED.,.F.,.F.,(4,1,1,1,1,1,
1,4),(40.8407044966672,41.2375488026267,42.2354663920146,43.2333839814026,
44.2313015707905,45.2292191601784,46.2271367495664,47.1238898038468),
 .UNSPECIFIED.);
#567=B_SPLINE_CURVE_WITH_KNOTS('',3,(#35647,#35648,#35649,#35650,#35651,
#35652,#35653,#35654,#35655,#35656,#35657),.UNSPECIFIED.,.F.,.F.,(4,1,1,
1,1,1,1,1,4),(34.5575191894876,34.567238170372,35.56515575976,36.5630733491479,
37.5609909385358,38.5589085279238,39.5568261173117,40.5547437066997,40.8407044966672),
 .UNSPECIFIED.);
#568=B_SPLINE_CURVE_WITH_KNOTS('',3,(#35658,#35659,#35660,#35661,#35662,
#35663,#35664,#35665,#35666,#35667),.UNSPECIFIED.,.F.,.F.,(4,1,1,1,1,1,
1,4),(34.5575191894876,35.2500432662991,36.247960855687,37.245878445075,
38.2437960344629,39.2417136238508,40.2396312132388,40.8407044966672),
 .UNSPECIFIED.);
#569=B_SPLINE_CURVE_WITH_KNOTS('',3,(#35672,#35673,#35674,#35675,#35676,
#35677,#35678,#35679,#35680,#35681),.UNSPECIFIED.,.F.,.F.,(4,1,1,1,1,1,
1,4),(28.2743338823081,28.5797326340444,29.5776502234324,30.5755678128203,
31.5734854022082,32.5714029915962,33.5693205809841,34.5575191894876),
 .UNSPECIFIED.);
#570=B_SPLINE_CURVE_WITH_KNOTS('',3,(#35682,#35683,#35684,#35685,#35686,
#35687,#35688,#35689,#35690,#35691),.UNSPECIFIED.,.F.,.F.,(4,1,1,1,1,1,
1,4),(28.2743338823081,29.2625377299715,30.2604553193594,31.2583729087473,
32.2562904981353,33.2542080875232,34.2521256769111,34.5575191894876),
 .UNSPECIFIED.);
#571=B_SPLINE_CURVE_WITH_KNOTS('',3,(#35696,#35697,#35698,#35699,#35700,
#35701,#35702,#35703,#35704,#35705),.UNSPECIFIED.,.F.,.F.,(4,1,1,1,1,1,
1,4),(21.9911485751285,22.5922270977168,23.5901446871048,24.5880622764927,
25.5859798658806,26.5838974552686,27.5818150446565,28.2743338823081),
 .UNSPECIFIED.);
#572=B_SPLINE_CURVE_WITH_KNOTS('',3,(#35706,#35707,#35708,#35709,#35710,
#35711,#35712,#35713,#35714,#35715,#35716),.UNSPECIFIED.,.F.,.F.,(4,1,1,
1,1,1,1,1,4),(21.9911485751285,22.2771146042559,23.2750321936439,24.2729497830318,
25.2708673724197,26.2687849618077,27.2667025511956,28.2646201405835,28.2743338823081),
 .UNSPECIFIED.);
#573=B_SPLINE_CURVE_WITH_KNOTS('',3,(#35721,#35722,#35723,#35724,#35725,
#35726,#35727,#35728,#35729,#35730),.UNSPECIFIED.,.F.,.F.,(4,1,1,1,1,1,
1,4),(15.7079632679489,16.6047215613892,17.6026391507771,18.6005567401651,
19.598474329553,20.5963919189409,21.5943095083289,21.9911485751285),
 .UNSPECIFIED.);
#574=B_SPLINE_CURVE_WITH_KNOTS('',3,(#35731,#35732,#35733,#35734,#35735,
#35736,#35737,#35738,#35739,#35740),.UNSPECIFIED.,.F.,.F.,(4,1,1,1,1,1,
1,4),(15.7079632679489,16.2896090679283,17.2875266573163,18.2854442467042,
19.2833618360921,20.2812794254801,21.279197014868,21.9911485751285),
 .UNSPECIFIED.);
#575=B_SPLINE_CURVE_WITH_KNOTS('',3,(#36198,#36199,#36200,#36201,#36202,
#36203,#36204,#36205,#36206,#36207,#36208,#36209,#36210,#36211,#36212,#36213,
#36214,#36215,#36216,#36217,#36218,#36219,#36220,#36221,#36222,#36223,#36224,
#36225,#36226,#36227,#36228,#36229,#36230,#36231,#36232,#36233,#36234,#36235,
#36236,#36237,#36238,#36239,#36240,#36241,#36242,#36243,#36244,#36245,#36246,
#36247,#36248,#36249,#36250,#36251,#36252,#36253,#36254,#36255,#36256,#36257,
#36258,#36259,#36260,#36261,#36262,#36263,#36264,#36265,#36266,#36267,#36268,
#36269,#36270,#36271,#36272,#36273,#36274,#36275,#36276,#36277,#36278,#36279),
 .UNSPECIFIED.,.F.,.F.,(4,3,3,3,3,3,3,3,3,3,3,3,3,3,3,3,3,3,3,3,3,3,3,3,
3,3,3,4),(-0.226379821609609,-0.217417340914373,-0.203083213732059,-0.195372161893588,
-0.192039947119467,-0.177142411517304,-0.167842650509623,-0.163493959889746,
-0.160580088349981,-0.14612114712645,-0.132066803420463,-0.124736183429312,
-0.120417462119026,-0.117749049396246,-0.10410960904933,-0.10274432345586,
-0.0897927198647197,-0.0833430124220497,-0.0779132429380391,-0.0753020462900725,
-0.0617532421277136,-0.0483128407128765,-0.0422737356237669,-0.0385418519188507,
-0.0362561171872797,-0.0233422370406623,-0.010890275470702,0.),
 .UNSPECIFIED.);
#576=B_SPLINE_CURVE_WITH_KNOTS('',3,(#36280,#36281,#36282,#36283),
 .UNSPECIFIED.,.F.,.F.,(4,4),(107.932659829997,108.699105814207),
 .UNSPECIFIED.);
#577=B_SPLINE_CURVE_WITH_KNOTS('',3,(#36285,#36286,#36287,#36288,#36289,
#36290,#36291,#36292,#36293,#36294,#36295,#36296,#36297,#36298,#36299,#36300,
#36301,#36302,#36303,#36304,#36305,#36306,#36307,#36308,#36309,#36310,#36311,
#36312,#36313,#36314,#36315,#36316,#36317,#36318,#36319,#36320,#36321,#36322,
#36323,#36324,#36325,#36326,#36327,#36328,#36329,#36330,#36331,#36332,#36333,
#36334,#36335,#36336,#36337,#36338,#36339,#36340,#36341,#36342,#36343,#36344,
#36345,#36346,#36347,#36348,#36349,#36350,#36351,#36352,#36353,#36354,#36355,
#36356,#36357,#36358,#36359,#36360,#36361,#36362,#36363,#36364,#36365,#36366),
 .UNSPECIFIED.,.F.,.F.,(4,3,3,3,3,3,3,3,3,3,3,3,3,3,3,3,3,3,3,3,3,3,3,3,
3,3,3,4),(-0.227523845437319,-0.220310172333792,-0.207301707943979,-0.203017170993446,
-0.199143852533238,-0.186050942785289,-0.177324882089039,-0.174438766917075,
-0.171551170337076,-0.15772399205663,-0.143919217003735,-0.137000027056623,
-0.134028108119541,-0.131666540053468,-0.11740868074808,-0.11624245721529,
-0.102496756909348,-0.0956119105440934,-0.0920583895072349,-0.0888709289525678,
-0.0745568929340286,-0.0599189450724288,-0.0524290769383752,-0.0472022677637861,
-0.0444388522067339,-0.0293009632710678,-0.0142728712478951,0.),
 .UNSPECIFIED.);
#578=B_SPLINE_CURVE_WITH_KNOTS('',3,(#36367,#36368,#36369,#36370,#36371,
#36372,#36373,#36374,#36375),.UNSPECIFIED.,.F.,.F.,(4,1,1,1,1,1,4),(10.3760149606788,
11.3000211209886,12.2979387103766,13.2958562997645,14.2937738891524,15.2916914785404,
15.7079632679489),.UNSPECIFIED.);
#579=B_SPLINE_CURVE_WITH_KNOTS('',3,(#36381,#36382,#36383,#36384,#36385,
#36386,#36387,#36388,#36389,#36390,#36391,#36392,#36393,#36394,#36395,#36396,
#36397,#36398,#36399,#36400,#36401,#36402,#36403,#36404,#36405,#36406,#36407,
#36408,#36409,#36410,#36411,#36412,#36413,#36414,#36415,#36416,#36417,#36418,
#36419,#36420,#36421,#36422,#36423,#36424,#36425,#36426,#36427,#36428,#36429,
#36430,#36431,#36432,#36433,#36434,#36435,#36436,#36437,#36438,#36439,#36440,
#36441,#36442,#36443,#36444,#36445,#36446,#36447,#36448,#36449,#36450,#36451,
#36452,#36453,#36454,#36455,#36456,#36457,#36458,#36459,#36460,#36461,#36462),
 .UNSPECIFIED.,.F.,.F.,(4,3,3,3,3,3,3,3,3,3,3,3,3,3,3,3,3,3,3,3,3,3,3,3,
3,3,3,4),(-0.226379821609595,-0.217417340914356,-0.203083213732043,-0.195372160903899,
-0.192039946137513,-0.17714241040132,-0.167842649533136,-0.163493952881452,
-0.16058007692827,-0.146121138560165,-0.132066791448452,-0.124736174450301,
-0.12041746383325,-0.117749050048006,-0.10410960636557,-0.10274432345585,
-0.089792743953128,-0.0833430503489106,-0.0779136525561493,-0.0753021579254146,
-0.0617533538087251,-0.048312953095273,-0.0422738339583639,-0.0385420785344113,
-0.0362564590884195,-0.023342576751842,-0.0108906149115675,0.),
 .UNSPECIFIED.);
#580=B_SPLINE_CURVE_WITH_KNOTS('',3,(#36465,#36466,#36467,#36468,#36469,
#36470,#36471,#36472),.UNSPECIFIED.,.F.,.F.,(4,1,1,1,1,4),(11.6151336144495,
12.6130512038375,13.6109687932254,14.6088863826133,15.6068039720013,15.7079632679489),
 .UNSPECIFIED.);
#581=B_SPLINE_CURVE_WITH_KNOTS('',3,(#36929,#36930,#36931,#36932,#36933,
#36934,#36935,#36936,#36937,#36938,#36939,#36940,#36941,#36942,#36943,#36944,
#36945,#36946,#36947,#36948,#36949,#36950,#36951,#36952,#36953,#36954,#36955,
#36956,#36957,#36958,#36959,#36960,#36961,#36962,#36963,#36964,#36965,#36966,
#36967,#36968,#36969,#36970,#36971,#36972,#36973,#36974,#36975,#36976,#36977,
#36978,#36979,#36980,#36981,#36982,#36983,#36984,#36985,#36986,#36987,#36988,
#36989,#36990,#36991,#36992,#36993,#36994,#36995,#36996,#36997,#36998,#36999,
#37000,#37001,#37002,#37003,#37004,#37005,#37006,#37007,#37008,#37009,#37010),
 .UNSPECIFIED.,.F.,.F.,(4,3,3,3,3,3,3,3,3,3,3,3,3,3,3,3,3,3,3,3,3,3,3,3,
3,3,3,4),(-0.227523845437348,-0.220310172333817,-0.207301707944002,-0.203017167295075,
-0.199143851355958,-0.186050939006339,-0.177324878782459,-0.174438745964263,
-0.171551166758963,-0.157723989373046,-0.143919214553493,-0.137000025218943,
-0.134028090264727,-0.131666515493408,-0.117408656293409,-0.116242457215294,
-0.102496755730857,-0.095611910182722,-0.0920583897601093,-0.0888709292326105,
-0.074556891706031,-0.0599189423638804,-0.0524290745683954,-0.0472022713413162,
-0.0444388545478162,-0.0293009645371915,-0.0142728755519417,0.),
 .UNSPECIFIED.);
#582=B_SPLINE_CURVE_WITH_KNOTS('',3,(#37019,#37020,#37021,#37022,#37023,
#37024),.UNSPECIFIED.,.F.,.F.,(4,2,4),(0.678296822341137,0.719813557564313,
0.76133029278749),.UNSPECIFIED.);
#583=B_SPLINE_CURVE_WITH_KNOTS('',3,(#37032,#37033,#37034,#37035,#37036,
#37037),.UNSPECIFIED.,.F.,.F.,(4,2,4),(0.678296822341137,0.719813557564313,
0.761330292787489),.UNSPECIFIED.);
#584=B_SPLINE_CURVE_WITH_KNOTS('',3,(#37043,#37044,#37045,#37046,#37047,
#37048),.UNSPECIFIED.,.F.,.F.,(4,2,4),(0.678296822341137,0.719813557564313,
0.76133029278749),.UNSPECIFIED.);
#585=B_SPLINE_CURVE_WITH_KNOTS('',3,(#37054,#37055,#37056,#37057,#37058,
#37059),.UNSPECIFIED.,.F.,.F.,(4,2,4),(0.678296822341137,0.719813557564313,
0.76133029278749),.UNSPECIFIED.);
#586=B_SPLINE_CURVE_WITH_KNOTS('',3,(#37065,#37066,#37067,#37068,#37069,
#37070),.UNSPECIFIED.,.F.,.F.,(4,2,4),(0.678296822341137,0.719813557564313,
0.76133029278749),.UNSPECIFIED.);
#587=B_SPLINE_CURVE_WITH_KNOTS('',3,(#37075,#37076,#37077,#37078,#37079,
#37080),.UNSPECIFIED.,.F.,.F.,(4,2,4),(0.678296822341137,0.719813557564313,
0.76133029278749),.UNSPECIFIED.);
#588=SHAPE_REPRESENTATION_RELATIONSHIP('SRR','None',#37238,#601);
#589=SHAPE_REPRESENTATION_RELATIONSHIP('SRR','None',#37239,#602);
#590=SHAPE_REPRESENTATION_RELATIONSHIP('SRR','None',#37240,#603);
#591=SHAPE_REPRESENTATION_RELATIONSHIP('SRR','None',#37241,#604);
#592=SHAPE_REPRESENTATION_RELATIONSHIP('SRR','None',#37242,#605);
#593=SHAPE_REPRESENTATION_RELATIONSHIP('SRR','None',#37243,#606);
#594=SHAPE_REPRESENTATION_RELATIONSHIP('SRR','None',#37244,#607);
#595=SHAPE_REPRESENTATION_RELATIONSHIP('SRR','None',#37245,#608);
#596=SHAPE_REPRESENTATION_RELATIONSHIP('SRR','None',#37246,#609);
#597=SHAPE_REPRESENTATION_RELATIONSHIP('SRR','None',#37247,#610);
#598=SHAPE_REPRESENTATION_RELATIONSHIP('SRR','None',#37248,#611);
#599=SHAPE_REPRESENTATION_RELATIONSHIP('SRR','None',#37249,#612);
#600=SHAPE_REPRESENTATION_RELATIONSHIP('SRR','None',#37250,#613);
#601=ADVANCED_BREP_SHAPE_REPRESENTATION('',(#627),#37168);
#602=ADVANCED_BREP_SHAPE_REPRESENTATION('',(#628),#37169);
#603=ADVANCED_BREP_SHAPE_REPRESENTATION('',(#629),#37170);
#604=ADVANCED_BREP_SHAPE_REPRESENTATION('',(#630),#37171);
#605=ADVANCED_BREP_SHAPE_REPRESENTATION('',(#631),#37172);
#606=ADVANCED_BREP_SHAPE_REPRESENTATION('',(#632),#37173);
#607=ADVANCED_BREP_SHAPE_REPRESENTATION('',(#633),#37174);
#608=ADVANCED_BREP_SHAPE_REPRESENTATION('',(#634),#37175);
#609=ADVANCED_BREP_SHAPE_REPRESENTATION('',(#635),#37176);
#610=ADVANCED_BREP_SHAPE_REPRESENTATION('',(#636),#37177);
#611=ADVANCED_BREP_SHAPE_REPRESENTATION('',(#637),#37178);
#612=ADVANCED_BREP_SHAPE_REPRESENTATION('',(#638),#37179);
#613=ADVANCED_BREP_SHAPE_REPRESENTATION('',(#639),#37180);
#614=STYLED_ITEM('',(#37359),#627);
#615=STYLED_ITEM('',(#37387),#628);
#616=STYLED_ITEM('',(#37352),#629);
#617=STYLED_ITEM('',(#37352),#630);
#618=STYLED_ITEM('',(#37387),#631);
#619=STYLED_ITEM('',(#37366),#632);
#620=STYLED_ITEM('',(#37387),#633);
#621=STYLED_ITEM('',(#37387),#634);
#622=STYLED_ITEM('',(#37380),#635);
#623=STYLED_ITEM('',(#37380),#636);
#624=STYLED_ITEM('',(#37380),#637);
#625=STYLED_ITEM('',(#37380),#638);
#626=STYLED_ITEM('',(#37380),#639);
#627=MANIFOLD_SOLID_BREP('Body1',#14776);
#628=MANIFOLD_SOLID_BREP('Body1',#14777);
#629=MANIFOLD_SOLID_BREP('Body1',#14778);
#630=MANIFOLD_SOLID_BREP('Body1',#14779);
#631=MANIFOLD_SOLID_BREP('Body1',#14780);
#632=MANIFOLD_SOLID_BREP('Body1',#14781);
#633=MANIFOLD_SOLID_BREP('Body1',#14782);
#634=MANIFOLD_SOLID_BREP('Body1',#14783);
#635=MANIFOLD_SOLID_BREP('Body1',#14784);
#636=MANIFOLD_SOLID_BREP('Body1',#14785);
#637=MANIFOLD_SOLID_BREP('Body1',#14786);
#638=MANIFOLD_SOLID_BREP('Body1',#14787);
#639=MANIFOLD_SOLID_BREP('Body1',#14788);
#640=FACE_BOUND('',#2226,.T.);
#641=FACE_BOUND('',#2241,.T.);
#642=FACE_BOUND('',#2250,.T.);
#643=FACE_BOUND('',#2253,.T.);
#644=FACE_BOUND('',#2261,.T.);
#645=FACE_BOUND('',#2293,.T.);
#646=FACE_BOUND('',#2303,.T.);
#647=FACE_BOUND('',#2305,.T.);
#648=FACE_BOUND('',#2313,.T.);
#649=FACE_BOUND('',#2321,.T.);
#650=FACE_BOUND('',#2336,.T.);
#651=FACE_BOUND('',#2339,.T.);
#652=FACE_BOUND('',#2351,.T.);
#653=FACE_BOUND('',#2354,.T.);
#654=FACE_BOUND('',#2365,.T.);
#655=FACE_BOUND('',#2382,.T.);
#656=FACE_BOUND('',#2386,.T.);
#657=FACE_BOUND('',#2389,.T.);
#658=FACE_BOUND('',#2401,.T.);
#659=FACE_BOUND('',#2415,.T.);
#660=FACE_BOUND('',#2446,.T.);
#661=FACE_BOUND('',#2457,.T.);
#662=FACE_BOUND('',#2484,.T.);
#663=FACE_BOUND('',#2485,.T.);
#664=FACE_BOUND('',#2502,.T.);
#665=FACE_BOUND('',#2517,.T.);
#666=FACE_BOUND('',#2518,.T.);
#667=FACE_BOUND('',#2519,.T.);
#668=FACE_BOUND('',#2522,.T.);
#669=FACE_BOUND('',#2523,.T.);
#670=FACE_BOUND('',#2524,.T.);
#671=FACE_BOUND('',#2587,.T.);
#672=FACE_BOUND('',#2588,.T.);
#673=FACE_BOUND('',#2589,.T.);
#674=FACE_BOUND('',#2614,.T.);
#675=FACE_BOUND('',#2617,.T.);
#676=FACE_BOUND('',#2678,.T.);
#677=FACE_BOUND('',#2784,.T.);
#678=FACE_BOUND('',#2790,.T.);
#679=FACE_BOUND('',#2829,.T.);
#680=FACE_BOUND('',#2840,.T.);
#681=FACE_BOUND('',#2937,.T.);
#682=FACE_BOUND('',#3006,.T.);
#683=FACE_BOUND('',#3011,.T.);
#684=FACE_BOUND('',#3017,.T.);
#685=FACE_BOUND('',#3020,.T.);
#686=FACE_BOUND('',#3028,.T.);
#687=FACE_BOUND('',#3031,.T.);
#688=FACE_BOUND('',#3090,.T.);
#689=FACE_BOUND('',#3095,.T.);
#690=CYLINDRICAL_SURFACE('',#14940,20.);
#691=CYLINDRICAL_SURFACE('',#14961,2.);
#692=CYLINDRICAL_SURFACE('',#14987,30.);
#693=CYLINDRICAL_SURFACE('',#14988,2.25);
#694=CYLINDRICAL_SURFACE('',#14990,2.25);
#695=CYLINDRICAL_SURFACE('',#14993,2.);
#696=CYLINDRICAL_SURFACE('',#15034,4.);
#697=CYLINDRICAL_SURFACE('',#15036,4.);
#698=CYLINDRICAL_SURFACE('',#15051,2.);
#699=CYLINDRICAL_SURFACE('',#15094,20.);
#700=CYLINDRICAL_SURFACE('',#15116,30.);
#701=CYLINDRICAL_SURFACE('',#15125,2.25);
#702=CYLINDRICAL_SURFACE('',#15126,2.25);
#703=CYLINDRICAL_SURFACE('',#15128,2.15);
#704=CYLINDRICAL_SURFACE('',#15130,2.15);
#705=CYLINDRICAL_SURFACE('',#15131,4.);
#706=CYLINDRICAL_SURFACE('',#15132,4.);
#707=CYLINDRICAL_SURFACE('',#15133,2.);
#708=CYLINDRICAL_SURFACE('',#15144,6.);
#709=CYLINDRICAL_SURFACE('',#15158,6.);
#710=CYLINDRICAL_SURFACE('',#15171,2.15);
#711=CYLINDRICAL_SURFACE('',#15177,2.15);
#712=CYLINDRICAL_SURFACE('',#15257,1.5);
#713=CYLINDRICAL_SURFACE('',#15261,1.5);
#714=CYLINDRICAL_SURFACE('',#15288,1.5);
#715=CYLINDRICAL_SURFACE('',#15290,1.5);
#716=CYLINDRICAL_SURFACE('',#15299,1.3);
#717=CYLINDRICAL_SURFACE('',#15303,1.3);
#718=CYLINDRICAL_SURFACE('',#15307,2.5);
#719=CYLINDRICAL_SURFACE('',#15327,4.2);
#720=CYLINDRICAL_SURFACE('',#15357,1.5);
#721=CYLINDRICAL_SURFACE('',#15360,1.5);
#722=CYLINDRICAL_SURFACE('',#15398,1.45);
#723=CYLINDRICAL_SURFACE('',#15399,1.45);
#724=CYLINDRICAL_SURFACE('',#15400,1.5);
#725=CYLINDRICAL_SURFACE('',#15401,1.5);
#726=CYLINDRICAL_SURFACE('',#15454,4.05);
#727=CYLINDRICAL_SURFACE('',#15456,3.954);
#728=CYLINDRICAL_SURFACE('',#15458,3.954);
#729=CYLINDRICAL_SURFACE('',#15459,3.954);
#730=CYLINDRICAL_SURFACE('',#15460,3.954);
#731=CYLINDRICAL_SURFACE('',#15461,3.954);
#732=CYLINDRICAL_SURFACE('',#15462,3.954);
#733=CYLINDRICAL_SURFACE('',#15463,3.954);
#734=CYLINDRICAL_SURFACE('',#15464,3.954);
#735=CYLINDRICAL_SURFACE('',#15465,3.954);
#736=CYLINDRICAL_SURFACE('',#15466,3.954);
#737=CYLINDRICAL_SURFACE('',#15467,3.954);
#738=CYLINDRICAL_SURFACE('',#15468,3.954);
#739=CYLINDRICAL_SURFACE('',#15469,3.954);
#740=CYLINDRICAL_SURFACE('',#15470,3.954);
#741=CYLINDRICAL_SURFACE('',#15471,3.954);
#742=CYLINDRICAL_SURFACE('',#15472,3.954);
#743=CYLINDRICAL_SURFACE('',#15473,3.954);
#744=CYLINDRICAL_SURFACE('',#15474,3.954);
#745=CYLINDRICAL_SURFACE('',#15475,3.954);
#746=CYLINDRICAL_SURFACE('',#15476,3.954);
#747=CYLINDRICAL_SURFACE('',#15477,3.954);
#748=CYLINDRICAL_SURFACE('',#15478,3.954);
#749=CYLINDRICAL_SURFACE('',#15479,3.954);
#750=CYLINDRICAL_SURFACE('',#15480,3.954);
#751=CYLINDRICAL_SURFACE('',#15481,3.954);
#752=CYLINDRICAL_SURFACE('',#15482,3.954);
#753=CYLINDRICAL_SURFACE('',#15483,3.954);
#754=CYLINDRICAL_SURFACE('',#15484,3.954);
#755=CYLINDRICAL_SURFACE('',#15485,3.52375);
#756=CYLINDRICAL_SURFACE('',#15487,3.52375);
#757=CYLINDRICAL_SURFACE('',#15488,3.52375);
#758=CYLINDRICAL_SURFACE('',#15489,3.52375);
#759=CYLINDRICAL_SURFACE('',#15490,3.52375);
#760=CYLINDRICAL_SURFACE('',#15491,3.52375);
#761=CYLINDRICAL_SURFACE('',#15492,3.52375);
#762=CYLINDRICAL_SURFACE('',#15493,3.52375);
#763=CYLINDRICAL_SURFACE('',#15494,3.52375);
#764=CYLINDRICAL_SURFACE('',#15495,3.52375);
#765=CYLINDRICAL_SURFACE('',#15496,3.52375);
#766=CYLINDRICAL_SURFACE('',#15497,3.52375);
#767=CYLINDRICAL_SURFACE('',#15498,3.52375);
#768=CYLINDRICAL_SURFACE('',#15499,3.52375);
#769=CYLINDRICAL_SURFACE('',#15500,3.52375);
#770=CYLINDRICAL_SURFACE('',#15501,3.52375);
#771=CYLINDRICAL_SURFACE('',#15502,3.52375);
#772=CYLINDRICAL_SURFACE('',#15503,3.52375);
#773=CYLINDRICAL_SURFACE('',#15504,3.52375);
#774=CYLINDRICAL_SURFACE('',#15505,3.52375);
#775=CYLINDRICAL_SURFACE('',#15506,3.52375);
#776=CYLINDRICAL_SURFACE('',#15507,3.52375);
#777=CYLINDRICAL_SURFACE('',#15508,3.52375);
#778=CYLINDRICAL_SURFACE('',#15509,3.52375);
#779=CYLINDRICAL_SURFACE('',#15510,3.52375);
#780=CYLINDRICAL_SURFACE('',#15511,3.52375);
#781=CYLINDRICAL_SURFACE('',#15512,3.52375);
#782=CYLINDRICAL_SURFACE('',#15564,5.);
#783=CYLINDRICAL_SURFACE('',#15597,3.52375);
#784=CYLINDRICAL_SURFACE('',#15697,3.954);
#785=CYLINDRICAL_SURFACE('',#15702,3.);
#786=CYLINDRICAL_SURFACE('',#15710,2.15);
#787=CYLINDRICAL_SURFACE('',#15715,6.5);
#788=CYLINDRICAL_SURFACE('',#15782,0.7);
#789=CYLINDRICAL_SURFACE('',#15802,0.7);
#790=CYLINDRICAL_SURFACE('',#15807,0.7);
#791=CYLINDRICAL_SURFACE('',#15808,0.7);
#792=CYLINDRICAL_SURFACE('',#15813,0.7);
#793=CYLINDRICAL_SURFACE('',#15814,0.7);
#794=CYLINDRICAL_SURFACE('',#15819,0.7);
#795=CYLINDRICAL_SURFACE('',#15820,0.7);
#796=CYLINDRICAL_SURFACE('',#15825,0.7);
#797=CYLINDRICAL_SURFACE('',#15826,0.7);
#798=CYLINDRICAL_SURFACE('',#15831,0.7);
#799=CYLINDRICAL_SURFACE('',#15832,0.7);
#800=CYLINDRICAL_SURFACE('',#15837,0.7);
#801=CYLINDRICAL_SURFACE('',#15838,0.7);
#802=CYLINDRICAL_SURFACE('',#15843,0.7);
#803=CYLINDRICAL_SURFACE('',#15844,0.7);
#804=CYLINDRICAL_SURFACE('',#15849,1.954);
#805=CYLINDRICAL_SURFACE('',#15851,1.954);
#806=CYLINDRICAL_SURFACE('',#15852,1.954);
#807=CYLINDRICAL_SURFACE('',#15853,1.954);
#808=CYLINDRICAL_SURFACE('',#15854,1.954);
#809=CYLINDRICAL_SURFACE('',#15855,1.954);
#810=CYLINDRICAL_SURFACE('',#15856,1.954);
#811=CYLINDRICAL_SURFACE('',#15857,1.954);
#812=CYLINDRICAL_SURFACE('',#15858,1.954);
#813=CYLINDRICAL_SURFACE('',#15859,1.954);
#814=CYLINDRICAL_SURFACE('',#15860,1.954);
#815=CYLINDRICAL_SURFACE('',#15861,1.954);
#816=CYLINDRICAL_SURFACE('',#15862,1.954);
#817=CYLINDRICAL_SURFACE('',#15863,1.954);
#818=CYLINDRICAL_SURFACE('',#15864,1.954);
#819=CYLINDRICAL_SURFACE('',#15865,1.954);
#820=CYLINDRICAL_SURFACE('',#15866,1.954);
#821=CYLINDRICAL_SURFACE('',#15867,1.954);
#822=CYLINDRICAL_SURFACE('',#15868,1.954);
#823=CYLINDRICAL_SURFACE('',#15869,1.954);
#824=CYLINDRICAL_SURFACE('',#15870,1.954);
#825=CYLINDRICAL_SURFACE('',#15871,1.954);
#826=CYLINDRICAL_SURFACE('',#15872,1.954);
#827=CYLINDRICAL_SURFACE('',#15873,1.5555);
#828=CYLINDRICAL_SURFACE('',#15875,1.5555);
#829=CYLINDRICAL_SURFACE('',#15876,1.5555);
#830=CYLINDRICAL_SURFACE('',#15877,1.5555);
#831=CYLINDRICAL_SURFACE('',#15878,1.5555);
#832=CYLINDRICAL_SURFACE('',#15879,1.5555);
#833=CYLINDRICAL_SURFACE('',#15880,1.5555);
#834=CYLINDRICAL_SURFACE('',#15881,1.5555);
#835=CYLINDRICAL_SURFACE('',#15882,1.5555);
#836=CYLINDRICAL_SURFACE('',#15883,1.5555);
#837=CYLINDRICAL_SURFACE('',#15884,1.5555);
#838=CYLINDRICAL_SURFACE('',#15885,1.5555);
#839=CYLINDRICAL_SURFACE('',#15886,1.5555);
#840=CYLINDRICAL_SURFACE('',#15887,1.5555);
#841=CYLINDRICAL_SURFACE('',#15888,1.5555);
#842=CYLINDRICAL_SURFACE('',#15889,1.5555);
#843=CYLINDRICAL_SURFACE('',#15890,1.5555);
#844=CYLINDRICAL_SURFACE('',#15891,1.5555);
#845=CYLINDRICAL_SURFACE('',#15892,1.5555);
#846=CYLINDRICAL_SURFACE('',#15893,1.5555);
#847=CYLINDRICAL_SURFACE('',#15894,1.5555);
#848=CYLINDRICAL_SURFACE('',#15895,1.5555);
#849=CYLINDRICAL_SURFACE('',#15900,1.5555);
#850=CYLINDRICAL_SURFACE('',#15901,1.954);
#851=CYLINDRICAL_SURFACE('',#15917,1.954);
#852=CYLINDRICAL_SURFACE('',#15919,1.954);
#853=CYLINDRICAL_SURFACE('',#15920,1.954);
#854=CYLINDRICAL_SURFACE('',#15921,1.954);
#855=CYLINDRICAL_SURFACE('',#15922,1.954);
#856=CYLINDRICAL_SURFACE('',#15923,1.954);
#857=CYLINDRICAL_SURFACE('',#15924,1.954);
#858=CYLINDRICAL_SURFACE('',#15925,1.954);
#859=CYLINDRICAL_SURFACE('',#15926,1.954);
#860=CYLINDRICAL_SURFACE('',#15927,1.954);
#861=CYLINDRICAL_SURFACE('',#15928,1.954);
#862=CYLINDRICAL_SURFACE('',#15929,1.954);
#863=CYLINDRICAL_SURFACE('',#15930,1.954);
#864=CYLINDRICAL_SURFACE('',#15931,1.954);
#865=CYLINDRICAL_SURFACE('',#15932,1.954);
#866=CYLINDRICAL_SURFACE('',#15933,1.954);
#867=CYLINDRICAL_SURFACE('',#15934,1.954);
#868=CYLINDRICAL_SURFACE('',#15935,1.954);
#869=CYLINDRICAL_SURFACE('',#15936,1.954);
#870=CYLINDRICAL_SURFACE('',#15937,1.954);
#871=CYLINDRICAL_SURFACE('',#15938,1.954);
#872=CYLINDRICAL_SURFACE('',#15939,1.954);
#873=CYLINDRICAL_SURFACE('',#15940,1.954);
#874=CYLINDRICAL_SURFACE('',#15941,1.954);
#875=CYLINDRICAL_SURFACE('',#15942,1.954);
#876=CYLINDRICAL_SURFACE('',#15943,1.954);
#877=CYLINDRICAL_SURFACE('',#15944,1.954);
#878=CYLINDRICAL_SURFACE('',#15945,1.954);
#879=CYLINDRICAL_SURFACE('',#15946,1.5555);
#880=CYLINDRICAL_SURFACE('',#15948,1.5555);
#881=CYLINDRICAL_SURFACE('',#15949,1.5555);
#882=CYLINDRICAL_SURFACE('',#15950,1.5555);
#883=CYLINDRICAL_SURFACE('',#15951,1.5555);
#884=CYLINDRICAL_SURFACE('',#15952,1.5555);
#885=CYLINDRICAL_SURFACE('',#15953,1.5555);
#886=CYLINDRICAL_SURFACE('',#15954,1.5555);
#887=CYLINDRICAL_SURFACE('',#15955,1.5555);
#888=CYLINDRICAL_SURFACE('',#15956,1.5555);
#889=CYLINDRICAL_SURFACE('',#15957,1.5555);
#890=CYLINDRICAL_SURFACE('',#15958,1.5555);
#891=CYLINDRICAL_SURFACE('',#15959,1.5555);
#892=CYLINDRICAL_SURFACE('',#15960,1.5555);
#893=CYLINDRICAL_SURFACE('',#15961,1.5555);
#894=CYLINDRICAL_SURFACE('',#15962,1.5555);
#895=CYLINDRICAL_SURFACE('',#15963,1.5555);
#896=CYLINDRICAL_SURFACE('',#15964,1.5555);
#897=CYLINDRICAL_SURFACE('',#15965,1.5555);
#898=CYLINDRICAL_SURFACE('',#15966,1.5555);
#899=CYLINDRICAL_SURFACE('',#15967,1.5555);
#900=CYLINDRICAL_SURFACE('',#15968,1.5555);
#901=CYLINDRICAL_SURFACE('',#15969,1.5555);
#902=CYLINDRICAL_SURFACE('',#15970,1.5555);
#903=CYLINDRICAL_SURFACE('',#15971,1.5555);
#904=CYLINDRICAL_SURFACE('',#15972,1.5555);
#905=CYLINDRICAL_SURFACE('',#15973,1.5555);
#906=CYLINDRICAL_SURFACE('',#15974,1.5555);
#907=CYLINDRICAL_SURFACE('',#15979,1.5555);
#908=CYLINDRICAL_SURFACE('',#15992,1.954);
#909=CYLINDRICAL_SURFACE('',#15996,3.8);
#910=CYLINDRICAL_SURFACE('',#16004,4.5);
#911=CYLINDRICAL_SURFACE('',#16008,2.2);
#912=CYLINDRICAL_SURFACE('',#16021,2.05);
#913=CYLINDRICAL_SURFACE('',#16040,1.215);
#914=CYLINDRICAL_SURFACE('',#16042,1.215);
#915=CYLINDRICAL_SURFACE('',#16043,1.215);
#916=CYLINDRICAL_SURFACE('',#16044,1.215);
#917=CYLINDRICAL_SURFACE('',#16045,1.215);
#918=CYLINDRICAL_SURFACE('',#16046,1.215);
#919=CYLINDRICAL_SURFACE('',#16047,1.215);
#920=CYLINDRICAL_SURFACE('',#16048,1.215);
#921=CYLINDRICAL_SURFACE('',#16049,1.215);
#922=CYLINDRICAL_SURFACE('',#16050,1.215);
#923=CYLINDRICAL_SURFACE('',#16051,1.215);
#924=CYLINDRICAL_SURFACE('',#16052,1.215);
#925=CYLINDRICAL_SURFACE('',#16053,1.215);
#926=CYLINDRICAL_SURFACE('',#16054,1.215);
#927=CYLINDRICAL_SURFACE('',#16055,1.215);
#928=CYLINDRICAL_SURFACE('',#16056,1.215);
#929=CYLINDRICAL_SURFACE('',#16057,1.215);
#930=CYLINDRICAL_SURFACE('',#16058,1.215);
#931=CYLINDRICAL_SURFACE('',#16060,0.95825);
#932=CYLINDRICAL_SURFACE('',#16062,0.95825);
#933=CYLINDRICAL_SURFACE('',#16063,0.95825);
#934=CYLINDRICAL_SURFACE('',#16064,0.95825);
#935=CYLINDRICAL_SURFACE('',#16065,0.95825);
#936=CYLINDRICAL_SURFACE('',#16066,0.95825);
#937=CYLINDRICAL_SURFACE('',#16067,0.95825);
#938=CYLINDRICAL_SURFACE('',#16068,0.95825);
#939=CYLINDRICAL_SURFACE('',#16069,0.95825);
#940=CYLINDRICAL_SURFACE('',#16070,0.95825);
#941=CYLINDRICAL_SURFACE('',#16071,0.95825);
#942=CYLINDRICAL_SURFACE('',#16072,0.95825);
#943=CYLINDRICAL_SURFACE('',#16073,0.95825);
#944=CYLINDRICAL_SURFACE('',#16074,0.95825);
#945=CYLINDRICAL_SURFACE('',#16075,0.95825);
#946=CYLINDRICAL_SURFACE('',#16076,0.95825);
#947=CYLINDRICAL_SURFACE('',#16077,0.95825);
#948=CYLINDRICAL_SURFACE('',#16082,0.95825);
#949=CYLINDRICAL_SURFACE('',#16095,1.215);
#950=CYLINDRICAL_SURFACE('',#16099,2.35);
#951=CIRCLE('',#14938,20.);
#952=CIRCLE('',#14939,20.5);
#953=CIRCLE('',#14941,20.);
#954=CIRCLE('',#14946,2.);
#955=CIRCLE('',#14947,1.52);
#956=CIRCLE('',#14953,2.);
#957=CIRCLE('',#14954,1.52);
#958=CIRCLE('',#14957,29.5);
#959=CIRCLE('',#14958,1.52);
#960=CIRCLE('',#14959,20.5);
#961=CIRCLE('',#14963,2.25);
#962=CIRCLE('',#14971,2.);
#963=CIRCLE('',#14976,2.);
#964=CIRCLE('',#14977,1.52);
#965=CIRCLE('',#14981,2.25);
#966=CIRCLE('',#14983,30.);
#967=CIRCLE('',#14985,30.);
#968=CIRCLE('',#14986,29.5);
#969=CIRCLE('',#14989,2.25);
#970=CIRCLE('',#14991,2.25);
#971=CIRCLE('',#15000,4.);
#972=CIRCLE('',#15001,3.52);
#973=CIRCLE('',#15004,4.);
#974=CIRCLE('',#15005,3.52);
#975=CIRCLE('',#15009,2.15);
#976=CIRCLE('',#15015,2.);
#977=CIRCLE('',#15016,1.52);
#978=CIRCLE('',#15019,4.);
#979=CIRCLE('',#15020,3.52);
#980=CIRCLE('',#15023,4.);
#981=CIRCLE('',#15024,3.52);
#982=CIRCLE('',#15027,2.);
#983=CIRCLE('',#15028,1.52);
#984=CIRCLE('',#15031,29.5);
#985=CIRCLE('',#15032,1.52);
#986=CIRCLE('',#15033,20.5);
#987=CIRCLE('',#15038,20.5);
#988=CIRCLE('',#15039,1.52);
#989=CIRCLE('',#15040,29.5);
#990=CIRCLE('',#15048,2.);
#991=CIRCLE('',#15052,2.);
#992=CIRCLE('',#15057,2.25);
#993=CIRCLE('',#15063,4.);
#994=CIRCLE('',#15064,3.52);
#995=CIRCLE('',#15067,4.);
#996=CIRCLE('',#15068,3.52);
#997=CIRCLE('',#15071,2.25);
#998=CIRCLE('',#15073,2.15);
#999=CIRCLE('',#15077,4.);
#1000=CIRCLE('',#15078,3.52);
#1001=CIRCLE('',#15081,4.);
#1002=CIRCLE('',#15082,3.52);
#1003=CIRCLE('',#15085,2.15);
#1004=CIRCLE('',#15090,20.);
#1005=CIRCLE('',#15093,20.);
#1006=CIRCLE('',#15095,20.);
#1007=CIRCLE('',#15096,20.);
#1008=CIRCLE('',#15101,20.48);
#1009=CIRCLE('',#15103,20.48);
#1010=CIRCLE('',#15105,29.52);
#1011=CIRCLE('',#15110,30.);
#1012=CIRCLE('',#15112,30.);
#1013=CIRCLE('',#15113,29.52);
#1014=CIRCLE('',#15117,30.);
#1015=CIRCLE('',#15118,30.);
#1016=CIRCLE('',#15121,2.25);
#1017=CIRCLE('',#15127,2.25);
#1018=CIRCLE('',#15129,2.15);
#1019=CIRCLE('',#15140,5.5);
#1020=CIRCLE('',#15141,6.);
#1021=CIRCLE('',#15145,6.);
#1022=CIRCLE('',#15149,5.5);
#1023=CIRCLE('',#15154,5.5);
#1024=CIRCLE('',#15155,6.);
#1025=CIRCLE('',#15159,6.);
#1026=CIRCLE('',#15169,2.65);
#1027=CIRCLE('',#15170,2.15);
#1028=CIRCLE('',#15172,2.15);
#1029=CIRCLE('',#15175,2.65);
#1030=CIRCLE('',#15176,2.15);
#1031=CIRCLE('',#15178,2.15);
#1032=CIRCLE('',#15181,2.65);
#1033=CIRCLE('',#15193,2.65);
#1034=CIRCLE('',#15197,5.5);
#1035=CIRCLE('',#15239,1.8);
#1036=CIRCLE('',#15240,1.8);
#1037=CIRCLE('',#15243,1.5);
#1038=CIRCLE('',#15244,1.);
#1039=CIRCLE('',#15247,1.5);
#1040=CIRCLE('',#15248,1.);
#1041=CIRCLE('',#15251,1.5);
#1042=CIRCLE('',#15252,1.);
#1043=CIRCLE('',#15255,1.5);
#1044=CIRCLE('',#15256,1.);
#1045=CIRCLE('',#15258,1.5);
#1046=CIRCLE('',#15260,3.);
#1047=CIRCLE('',#15262,1.5);
#1048=CIRCLE('',#15269,1.5);
#1049=CIRCLE('',#15270,1.);
#1050=CIRCLE('',#15273,1.5);
#1051=CIRCLE('',#15274,1.);
#1052=CIRCLE('',#15277,1.);
#1053=CIRCLE('',#15280,1.);
#1054=CIRCLE('',#15297,1.3);
#1055=CIRCLE('',#15298,1.3);
#1056=CIRCLE('',#15300,1.3);
#1057=CIRCLE('',#15302,1.3);
#1058=CIRCLE('',#15304,1.3);
#1059=CIRCLE('',#15306,2.5);
#1060=CIRCLE('',#15308,2.5);
#1061=CIRCLE('',#15310,3.);
#1062=CIRCLE('',#15325,4.4);
#1063=CIRCLE('',#15326,4.2);
#1064=CIRCLE('',#15328,4.2);
#1065=CIRCLE('',#15330,1.30000000000001);
#1066=CIRCLE('',#15331,1.30000000000001);
#1067=CIRCLE('',#15332,1.30000000000001);
#1068=CIRCLE('',#15333,1.3);
#1069=CIRCLE('',#15334,1.45);
#1070=CIRCLE('',#15335,1.45);
#1071=CIRCLE('',#15337,4.4);
#1072=CIRCLE('',#15339,0.800000000000008);
#1073=CIRCLE('',#15340,0.800000000000008);
#1074=CIRCLE('',#15341,0.80000000000001);
#1075=CIRCLE('',#15342,0.800000000000012);
#1076=CIRCLE('',#15343,1.45);
#1077=CIRCLE('',#15344,1.45);
#1078=CIRCLE('',#15347,1.5);
#1079=CIRCLE('',#15350,1.5);
#1080=CIRCLE('',#15353,1.5);
#1081=CIRCLE('',#15356,1.5);
#1082=CIRCLE('',#15358,1.5);
#1083=CIRCLE('',#15361,1.5);
#1084=CIRCLE('',#15365,1.35857864376269);
#1085=CIRCLE('',#15368,1.35857864376269);
#1086=CIRCLE('',#15371,1.3585786437627);
#1087=CIRCLE('',#15372,1.5);
#1088=CIRCLE('',#15375,1.35857864376269);
#1089=CIRCLE('',#15376,1.5);
#1090=CIRCLE('',#15378,1.14142135623731);
#1091=CIRCLE('',#15381,1.14142135623731);
#1092=CIRCLE('',#15390,1.1414213562373);
#1093=CIRCLE('',#15393,1.1414213562373);
#1094=CIRCLE('',#15449,4.05);
#1095=CIRCLE('',#15452,4.05);
#1096=CIRCLE('',#15457,3.954);
#1097=CIRCLE('',#15486,3.52375);
#1098=CIRCLE('',#15514,5.);
#1099=CIRCLE('',#15515,4.6);
#1100=CIRCLE('',#15516,5.);
#1101=CIRCLE('',#15517,5.);
#1102=CIRCLE('',#15518,5.);
#1103=CIRCLE('',#15519,5.);
#1104=CIRCLE('',#15520,5.);
#1105=CIRCLE('',#15521,5.);
#1106=CIRCLE('',#15522,5.);
#1107=CIRCLE('',#15523,5.);
#1108=CIRCLE('',#15524,5.);
#1109=CIRCLE('',#15525,5.);
#1110=CIRCLE('',#15526,5.);
#1111=CIRCLE('',#15527,5.);
#1112=CIRCLE('',#15528,5.);
#1113=CIRCLE('',#15529,5.);
#1114=CIRCLE('',#15530,5.);
#1115=CIRCLE('',#15531,5.);
#1116=CIRCLE('',#15532,5.);
#1117=CIRCLE('',#15533,5.);
#1118=CIRCLE('',#15534,5.);
#1119=CIRCLE('',#15535,5.);
#1120=CIRCLE('',#15536,5.);
#1121=CIRCLE('',#15537,5.);
#1122=CIRCLE('',#15538,5.);
#1123=CIRCLE('',#15539,5.);
#1124=CIRCLE('',#15540,5.);
#1125=CIRCLE('',#15541,5.);
#1126=CIRCLE('',#15542,5.);
#1127=CIRCLE('',#15543,5.);
#1128=CIRCLE('',#15544,5.);
#1129=CIRCLE('',#15545,5.);
#1130=CIRCLE('',#15546,5.);
#1131=CIRCLE('',#15547,5.);
#1132=CIRCLE('',#15548,5.);
#1133=CIRCLE('',#15549,5.);
#1134=CIRCLE('',#15550,5.);
#1135=CIRCLE('',#15551,5.);
#1136=CIRCLE('',#15552,5.);
#1137=CIRCLE('',#15553,5.);
#1138=CIRCLE('',#15554,5.);
#1139=CIRCLE('',#15555,5.);
#1140=CIRCLE('',#15556,5.);
#1141=CIRCLE('',#15557,5.);
#1142=CIRCLE('',#15558,5.);
#1143=CIRCLE('',#15559,5.);
#1144=CIRCLE('',#15560,5.);
#1145=CIRCLE('',#15561,5.);
#1146=CIRCLE('',#15562,5.);
#1147=CIRCLE('',#15563,5.);
#1148=CIRCLE('',#15565,5.);
#1149=CIRCLE('',#15566,5.);
#1150=CIRCLE('',#15567,5.);
#1151=CIRCLE('',#15568,5.);
#1152=CIRCLE('',#15569,5.);
#1153=CIRCLE('',#15570,5.);
#1154=CIRCLE('',#15571,5.);
#1155=CIRCLE('',#15572,5.);
#1156=CIRCLE('',#15573,5.);
#1157=CIRCLE('',#15574,5.);
#1158=CIRCLE('',#15575,5.);
#1159=CIRCLE('',#15576,5.);
#1160=CIRCLE('',#15577,5.);
#1161=CIRCLE('',#15578,5.);
#1162=CIRCLE('',#15579,5.);
#1163=CIRCLE('',#15580,5.);
#1164=CIRCLE('',#15581,5.);
#1165=CIRCLE('',#15582,5.);
#1166=CIRCLE('',#15583,5.);
#1167=CIRCLE('',#15584,5.);
#1168=CIRCLE('',#15585,5.);
#1169=CIRCLE('',#15586,5.);
#1170=CIRCLE('',#15587,5.);
#1171=CIRCLE('',#15588,5.);
#1172=CIRCLE('',#15589,5.);
#1173=CIRCLE('',#15590,5.);
#1174=CIRCLE('',#15592,3.954);
#1175=CIRCLE('',#15594,3.954);
#1176=CIRCLE('',#15595,3.954);
#1177=CIRCLE('',#15596,3.52375);
#1178=CIRCLE('',#15695,3.6);
#1179=CIRCLE('',#15699,4.5);
#1180=CIRCLE('',#15701,3.);
#1181=CIRCLE('',#15703,3.);
#1182=CIRCLE('',#15707,2.15);
#1183=CIRCLE('',#15708,2.15);
#1184=CIRCLE('',#15709,2.47);
#1185=CIRCLE('',#15711,2.15);
#1186=CIRCLE('',#15713,5.9);
#1187=CIRCLE('',#15716,6.5);
#1188=CIRCLE('',#15717,6.5);
#1189=CIRCLE('',#15718,6.5);
#1190=CIRCLE('',#15719,6.5);
#1191=CIRCLE('',#15720,6.5);
#1192=CIRCLE('',#15721,6.5);
#1193=CIRCLE('',#15722,6.5);
#1194=CIRCLE('',#15723,6.5);
#1195=CIRCLE('',#15724,6.5);
#1196=CIRCLE('',#15725,6.5);
#1197=CIRCLE('',#15726,6.5);
#1198=CIRCLE('',#15727,6.5);
#1199=CIRCLE('',#15728,6.5);
#1200=CIRCLE('',#15729,6.5);
#1201=CIRCLE('',#15730,6.5);
#1202=CIRCLE('',#15731,6.5);
#1203=CIRCLE('',#15732,6.5);
#1204=CIRCLE('',#15733,6.5);
#1205=CIRCLE('',#15734,6.5);
#1206=CIRCLE('',#15735,6.5);
#1207=CIRCLE('',#15736,6.5);
#1208=CIRCLE('',#15737,6.5);
#1209=CIRCLE('',#15738,6.5);
#1210=CIRCLE('',#15739,6.5);
#1211=CIRCLE('',#15740,6.5);
#1212=CIRCLE('',#15741,6.5);
#1213=CIRCLE('',#15742,6.5);
#1214=CIRCLE('',#15743,6.5);
#1215=CIRCLE('',#15744,6.5);
#1216=CIRCLE('',#15745,6.5);
#1217=CIRCLE('',#15746,6.5);
#1218=CIRCLE('',#15747,6.5);
#1219=CIRCLE('',#15748,6.5);
#1220=CIRCLE('',#15749,6.5);
#1221=CIRCLE('',#15783,0.7);
#1222=CIRCLE('',#15785,2.47);
#1223=CIRCLE('',#15797,6.);
#1224=CIRCLE('',#15803,0.7);
#1225=CIRCLE('',#15806,0.7);
#1226=CIRCLE('',#15809,0.7);
#1227=CIRCLE('',#15812,0.7);
#1228=CIRCLE('',#15815,0.7);
#1229=CIRCLE('',#15818,0.7);
#1230=CIRCLE('',#15821,0.7);
#1231=CIRCLE('',#15824,0.7);
#1232=CIRCLE('',#15827,0.7);
#1233=CIRCLE('',#15830,0.7);
#1234=CIRCLE('',#15833,0.7);
#1235=CIRCLE('',#15836,0.7);
#1236=CIRCLE('',#15839,0.7);
#1237=CIRCLE('',#15842,0.7);
#1238=CIRCLE('',#15845,0.7);
#1239=CIRCLE('',#15850,1.954);
#1240=CIRCLE('',#15874,1.5555);
#1241=CIRCLE('',#15897,1.954);
#1242=CIRCLE('',#15898,1.954);
#1243=CIRCLE('',#15899,1.5555);
#1244=CIRCLE('',#15902,1.954);
#1245=CIRCLE('',#15904,1.6);
#1246=CIRCLE('',#15907,3.34203030879952);
#1247=CIRCLE('',#15918,1.954);
#1248=CIRCLE('',#15947,1.5555);
#1249=CIRCLE('',#15976,1.954);
#1250=CIRCLE('',#15977,1.954);
#1251=CIRCLE('',#15978,1.5555);
#1252=CIRCLE('',#15981,1.23357587978679);
#1253=CIRCLE('',#15990,1.6);
#1254=CIRCLE('',#15993,1.954);
#1255=CIRCLE('',#15995,3.8);
#1256=CIRCLE('',#15997,3.8);
#1257=CIRCLE('',#15998,3.8);
#1258=CIRCLE('',#16001,4.3);
#1259=CIRCLE('',#16002,4.5);
#1260=CIRCLE('',#16003,4.5);
#1261=CIRCLE('',#16005,4.5);
#1262=CIRCLE('',#16007,2.2);
#1263=CIRCLE('',#16009,2.2);
#1264=CIRCLE('',#16011,4.35);
#1265=CIRCLE('',#16017,3.34203030879952);
#1266=CIRCLE('',#16019,2.25);
#1267=CIRCLE('',#16020,2.05);
#1268=CIRCLE('',#16022,2.05);
#1269=CIRCLE('',#16024,3.34203030879952);
#1270=CIRCLE('',#16026,2.25);
#1271=CIRCLE('',#16041,1.215);
#1272=CIRCLE('',#16059,1.215);
#1273=CIRCLE('',#16061,0.95825);
#1274=CIRCLE('',#16079,1.215);
#1275=CIRCLE('',#16080,1.215);
#1276=CIRCLE('',#16081,0.95825);
#1277=CIRCLE('',#16084,0.733718498103797);
#1278=CIRCLE('',#16093,1.);
#1279=CIRCLE('',#16096,1.215);
#1280=CIRCLE('',#16098,2.35);
#1281=CIRCLE('',#16100,2.35);
#1282=CIRCLE('',#16101,2.35);
#1283=CONICAL_SURFACE('',#14937,20.25,0.785398163397446);
#1284=CONICAL_SURFACE('',#14945,1.76,0.78539816339745);
#1285=CONICAL_SURFACE('',#14952,1.76,0.78539816339745);
#1286=CONICAL_SURFACE('',#14970,1.76,0.785398163397452);
#1287=CONICAL_SURFACE('',#14975,1.76,0.785398163397452);
#1288=CONICAL_SURFACE('',#14979,20.25,0.785398163397446);
#1289=CONICAL_SURFACE('',#14982,29.75,0.785398163397446);
#1290=CONICAL_SURFACE('',#14984,29.75,0.785398163397446);
#1291=CONICAL_SURFACE('',#14999,3.76,0.785398163397446);
#1292=CONICAL_SURFACE('',#15003,3.76,0.785398163397446);
#1293=CONICAL_SURFACE('',#15014,1.76,0.78539816339745);
#1294=CONICAL_SURFACE('',#15018,3.76,0.785398163397446);
#1295=CONICAL_SURFACE('',#15022,3.76,0.785398163397446);
#1296=CONICAL_SURFACE('',#15026,1.76,0.78539816339745);
#1297=CONICAL_SURFACE('',#15047,1.76,0.785398163397452);
#1298=CONICAL_SURFACE('',#15059,1.76,0.785398163397452);
#1299=CONICAL_SURFACE('',#15062,3.76,0.785398163397446);
#1300=CONICAL_SURFACE('',#15066,3.76,0.785398163397446);
#1301=CONICAL_SURFACE('',#15076,3.76,0.785398163397446);
#1302=CONICAL_SURFACE('',#15080,3.76,0.785398163397446);
#1303=CONICAL_SURFACE('',#15089,20.25,0.785398163397446);
#1304=CONICAL_SURFACE('',#15092,20.25,0.785398163397446);
#1305=CONICAL_SURFACE('',#15100,20.24,0.785398163397448);
#1306=CONICAL_SURFACE('',#15102,20.24,0.785398163397449);
#1307=CONICAL_SURFACE('',#15109,29.76,0.785398163397449);
#1308=CONICAL_SURFACE('',#15111,29.76,0.785398163397448);
#1309=CONICAL_SURFACE('',#15119,29.75,0.785398163397446);
#1310=CONICAL_SURFACE('',#15122,29.75,0.785398163397446);
#1311=CONICAL_SURFACE('',#15139,5.75,0.785398163397448);
#1312=CONICAL_SURFACE('',#15148,5.75,0.785398163397448);
#1313=CONICAL_SURFACE('',#15153,5.75,0.785398163397448);
#1314=CONICAL_SURFACE('',#15168,2.4,0.785398163397448);
#1315=CONICAL_SURFACE('',#15174,2.4,0.785398163397448);
#1316=CONICAL_SURFACE('',#15180,2.4,0.785398163397448);
#1317=CONICAL_SURFACE('',#15192,2.4,0.785398163397448);
#1318=CONICAL_SURFACE('',#15196,5.75,0.785398163397448);
#1319=CONICAL_SURFACE('',#15242,1.25,0.785398163397451);
#1320=CONICAL_SURFACE('',#15246,1.25,0.785398163397449);
#1321=CONICAL_SURFACE('',#15250,1.25,0.785398163397449);
#1322=CONICAL_SURFACE('',#15254,1.25,0.785398163397451);
#1323=CONICAL_SURFACE('',#15268,1.25,0.785398163397451);
#1324=CONICAL_SURFACE('',#15272,1.25,0.785398163397449);
#1325=CONICAL_SURFACE('',#15276,1.25,0.785398163397449);
#1326=CONICAL_SURFACE('',#15279,1.25,0.785398163397451);
#1327=CONICAL_SURFACE('',#15296,1.55,0.785398163397446);
#1328=CONICAL_SURFACE('',#15301,1.55,0.785398163397446);
#1329=CONICAL_SURFACE('',#15305,2.75,0.785398163397448);
#1330=CONICAL_SURFACE('',#15309,2.75,0.785398163397448);
#1331=CONICAL_SURFACE('',#15324,4.3,0.785398163397448);
#1332=CONICAL_SURFACE('',#15336,4.3,0.785398163397448);
#1333=CONICAL_SURFACE('',#15346,1.4,0.785398163397434);
#1334=CONICAL_SURFACE('',#15349,1.4,0.785398163397434);
#1335=CONICAL_SURFACE('',#15352,1.4,0.785398163397435);
#1336=CONICAL_SURFACE('',#15355,1.4,0.785398163397443);
#1337=CONICAL_SURFACE('',#15364,1.42928932188135,0.392699081698732);
#1338=CONICAL_SURFACE('',#15367,1.42928932188135,0.392699081698732);
#1339=CONICAL_SURFACE('',#15370,1.42928932188135,0.392699081698704);
#1340=CONICAL_SURFACE('',#15374,1.42928932188135,0.392699081698719);
#1341=CONICAL_SURFACE('',#15377,1.25,0.785398163397447);
#1342=CONICAL_SURFACE('',#15380,1.25,0.785398163397444);
#1343=CONICAL_SURFACE('',#15385,0.970710678118663,1.17809724509616);
#1344=CONICAL_SURFACE('',#15387,0.97071067811866,1.17809724509617);
#1345=CONICAL_SURFACE('',#15389,0.970710678118656,1.17809724509617);
#1346=CONICAL_SURFACE('',#15392,0.970710678118656,1.17809724509617);
#1347=CONICAL_SURFACE('',#15394,1.25,0.785398163397447);
#1348=CONICAL_SURFACE('',#15396,1.25,0.785398163397447);
#1349=CONICAL_SURFACE('',#15513,4.8,0.785398163397448);
#1350=CONICAL_SURFACE('',#15696,3.8,0.785398163397448);
#1351=CONICAL_SURFACE('',#15698,4.75,0.785398163397446);
#1352=CONICAL_SURFACE('',#15706,2.31,0.785398163397448);
#1353=CONICAL_SURFACE('',#15750,6.2,0.785398163397447);
#1354=CONICAL_SURFACE('',#15784,2.31,0.785398163397448);
#1355=CONICAL_SURFACE('',#15847,6.25,0.785398163397449);
#1356=CONICAL_SURFACE('',#15905,1.8,0.785398163397448);
#1357=CONICAL_SURFACE('',#15906,3.83322594216369,1.03985037524359);
#1358=CONICAL_SURFACE('',#15980,0.625,1.02388712580674);
#1359=CONICAL_SURFACE('',#15991,1.8,0.785398163397451);
#1360=CONICAL_SURFACE('',#16000,4.4,0.785398163397449);
#1361=CONICAL_SURFACE('',#16012,4.425,0.785398163397451);
#1362=CONICAL_SURFACE('',#16016,3.83322594216369,1.03985037524359);
#1363=CONICAL_SURFACE('',#16018,2.15,0.785398163397448);
#1364=CONICAL_SURFACE('',#16025,2.15,0.785398163397448);
#1365=CONICAL_SURFACE('',#16030,3.83322594216369,1.03985037524359);
#1366=CONICAL_SURFACE('',#16083,0.375,1.02000541721991);
#1367=CONICAL_SURFACE('',#16094,1.125,0.785398163397448);
#1368=FACE_OUTER_BOUND('',#2208,.T.);
#1369=FACE_OUTER_BOUND('',#2209,.T.);
#1370=FACE_OUTER_BOUND('',#2210,.T.);
#1371=FACE_OUTER_BOUND('',#2211,.T.);
#1372=FACE_OUTER_BOUND('',#2212,.T.);
#1373=FACE_OUTER_BOUND('',#2213,.T.);
#1374=FACE_OUTER_BOUND('',#2214,.T.);
#1375=FACE_OUTER_BOUND('',#2215,.T.);
#1376=FACE_OUTER_BOUND('',#2216,.T.);
#1377=FACE_OUTER_BOUND('',#2217,.T.);
#1378=FACE_OUTER_BOUND('',#2218,.T.);
#1379=FACE_OUTER_BOUND('',#2219,.T.);
#1380=FACE_OUTER_BOUND('',#2220,.T.);
#1381=FACE_OUTER_BOUND('',#2221,.T.);
#1382=FACE_OUTER_BOUND('',#2222,.T.);
#1383=FACE_OUTER_BOUND('',#2223,.T.);
#1384=FACE_OUTER_BOUND('',#2224,.T.);
#1385=FACE_OUTER_BOUND('',#2225,.T.);
#1386=FACE_OUTER_BOUND('',#2227,.T.);
#1387=FACE_OUTER_BOUND('',#2228,.T.);
#1388=FACE_OUTER_BOUND('',#2229,.T.);
#1389=FACE_OUTER_BOUND('',#2230,.T.);
#1390=FACE_OUTER_BOUND('',#2231,.T.);
#1391=FACE_OUTER_BOUND('',#2232,.T.);
#1392=FACE_OUTER_BOUND('',#2233,.T.);
#1393=FACE_OUTER_BOUND('',#2234,.T.);
#1394=FACE_OUTER_BOUND('',#2235,.T.);
#1395=FACE_OUTER_BOUND('',#2236,.T.);
#1396=FACE_OUTER_BOUND('',#2237,.T.);
#1397=FACE_OUTER_BOUND('',#2238,.T.);
#1398=FACE_OUTER_BOUND('',#2239,.T.);
#1399=FACE_OUTER_BOUND('',#2240,.T.);
#1400=FACE_OUTER_BOUND('',#2242,.T.);
#1401=FACE_OUTER_BOUND('',#2243,.T.);
#1402=FACE_OUTER_BOUND('',#2244,.T.);
#1403=FACE_OUTER_BOUND('',#2245,.T.);
#1404=FACE_OUTER_BOUND('',#2246,.T.);
#1405=FACE_OUTER_BOUND('',#2247,.T.);
#1406=FACE_OUTER_BOUND('',#2248,.T.);
#1407=FACE_OUTER_BOUND('',#2249,.T.);
#1408=FACE_OUTER_BOUND('',#2251,.T.);
#1409=FACE_OUTER_BOUND('',#2252,.T.);
#1410=FACE_OUTER_BOUND('',#2254,.T.);
#1411=FACE_OUTER_BOUND('',#2255,.T.);
#1412=FACE_OUTER_BOUND('',#2256,.T.);
#1413=FACE_OUTER_BOUND('',#2257,.T.);
#1414=FACE_OUTER_BOUND('',#2258,.T.);
#1415=FACE_OUTER_BOUND('',#2259,.T.);
#1416=FACE_OUTER_BOUND('',#2260,.T.);
#1417=FACE_OUTER_BOUND('',#2262,.T.);
#1418=FACE_OUTER_BOUND('',#2263,.T.);
#1419=FACE_OUTER_BOUND('',#2264,.T.);
#1420=FACE_OUTER_BOUND('',#2265,.T.);
#1421=FACE_OUTER_BOUND('',#2266,.T.);
#1422=FACE_OUTER_BOUND('',#2267,.T.);
#1423=FACE_OUTER_BOUND('',#2268,.T.);
#1424=FACE_OUTER_BOUND('',#2269,.T.);
#1425=FACE_OUTER_BOUND('',#2270,.T.);
#1426=FACE_OUTER_BOUND('',#2271,.T.);
#1427=FACE_OUTER_BOUND('',#2272,.T.);
#1428=FACE_OUTER_BOUND('',#2273,.T.);
#1429=FACE_OUTER_BOUND('',#2274,.T.);
#1430=FACE_OUTER_BOUND('',#2275,.T.);
#1431=FACE_OUTER_BOUND('',#2276,.T.);
#1432=FACE_OUTER_BOUND('',#2277,.T.);
#1433=FACE_OUTER_BOUND('',#2278,.T.);
#1434=FACE_OUTER_BOUND('',#2279,.T.);
#1435=FACE_OUTER_BOUND('',#2280,.T.);
#1436=FACE_OUTER_BOUND('',#2281,.T.);
#1437=FACE_OUTER_BOUND('',#2282,.T.);
#1438=FACE_OUTER_BOUND('',#2283,.T.);
#1439=FACE_OUTER_BOUND('',#2284,.T.);
#1440=FACE_OUTER_BOUND('',#2285,.T.);
#1441=FACE_OUTER_BOUND('',#2286,.T.);
#1442=FACE_OUTER_BOUND('',#2287,.T.);
#1443=FACE_OUTER_BOUND('',#2288,.T.);
#1444=FACE_OUTER_BOUND('',#2289,.T.);
#1445=FACE_OUTER_BOUND('',#2290,.T.);
#1446=FACE_OUTER_BOUND('',#2291,.T.);
#1447=FACE_OUTER_BOUND('',#2292,.T.);
#1448=FACE_OUTER_BOUND('',#2294,.T.);
#1449=FACE_OUTER_BOUND('',#2295,.T.);
#1450=FACE_OUTER_BOUND('',#2296,.T.);
#1451=FACE_OUTER_BOUND('',#2297,.T.);
#1452=FACE_OUTER_BOUND('',#2298,.T.);
#1453=FACE_OUTER_BOUND('',#2299,.T.);
#1454=FACE_OUTER_BOUND('',#2300,.T.);
#1455=FACE_OUTER_BOUND('',#2301,.T.);
#1456=FACE_OUTER_BOUND('',#2302,.T.);
#1457=FACE_OUTER_BOUND('',#2304,.T.);
#1458=FACE_OUTER_BOUND('',#2306,.T.);
#1459=FACE_OUTER_BOUND('',#2307,.T.);
#1460=FACE_OUTER_BOUND('',#2308,.T.);
#1461=FACE_OUTER_BOUND('',#2309,.T.);
#1462=FACE_OUTER_BOUND('',#2310,.T.);
#1463=FACE_OUTER_BOUND('',#2311,.T.);
#1464=FACE_OUTER_BOUND('',#2312,.T.);
#1465=FACE_OUTER_BOUND('',#2314,.T.);
#1466=FACE_OUTER_BOUND('',#2315,.T.);
#1467=FACE_OUTER_BOUND('',#2316,.T.);
#1468=FACE_OUTER_BOUND('',#2317,.T.);
#1469=FACE_OUTER_BOUND('',#2318,.T.);
#1470=FACE_OUTER_BOUND('',#2319,.T.);
#1471=FACE_OUTER_BOUND('',#2320,.T.);
#1472=FACE_OUTER_BOUND('',#2322,.T.);
#1473=FACE_OUTER_BOUND('',#2323,.T.);
#1474=FACE_OUTER_BOUND('',#2324,.T.);
#1475=FACE_OUTER_BOUND('',#2325,.T.);
#1476=FACE_OUTER_BOUND('',#2326,.T.);
#1477=FACE_OUTER_BOUND('',#2327,.T.);
#1478=FACE_OUTER_BOUND('',#2328,.T.);
#1479=FACE_OUTER_BOUND('',#2329,.T.);
#1480=FACE_OUTER_BOUND('',#2330,.T.);
#1481=FACE_OUTER_BOUND('',#2331,.T.);
#1482=FACE_OUTER_BOUND('',#2332,.T.);
#1483=FACE_OUTER_BOUND('',#2333,.T.);
#1484=FACE_OUTER_BOUND('',#2334,.T.);
#1485=FACE_OUTER_BOUND('',#2335,.T.);
#1486=FACE_OUTER_BOUND('',#2337,.T.);
#1487=FACE_OUTER_BOUND('',#2338,.T.);
#1488=FACE_OUTER_BOUND('',#2340,.T.);
#1489=FACE_OUTER_BOUND('',#2341,.T.);
#1490=FACE_OUTER_BOUND('',#2342,.T.);
#1491=FACE_OUTER_BOUND('',#2343,.T.);
#1492=FACE_OUTER_BOUND('',#2344,.T.);
#1493=FACE_OUTER_BOUND('',#2345,.T.);
#1494=FACE_OUTER_BOUND('',#2346,.T.);
#1495=FACE_OUTER_BOUND('',#2347,.T.);
#1496=FACE_OUTER_BOUND('',#2348,.T.);
#1497=FACE_OUTER_BOUND('',#2349,.T.);
#1498=FACE_OUTER_BOUND('',#2350,.T.);
#1499=FACE_OUTER_BOUND('',#2352,.T.);
#1500=FACE_OUTER_BOUND('',#2353,.T.);
#1501=FACE_OUTER_BOUND('',#2355,.T.);
#1502=FACE_OUTER_BOUND('',#2356,.T.);
#1503=FACE_OUTER_BOUND('',#2357,.T.);
#1504=FACE_OUTER_BOUND('',#2358,.T.);
#1505=FACE_OUTER_BOUND('',#2359,.T.);
#1506=FACE_OUTER_BOUND('',#2360,.T.);
#1507=FACE_OUTER_BOUND('',#2361,.T.);
#1508=FACE_OUTER_BOUND('',#2362,.T.);
#1509=FACE_OUTER_BOUND('',#2363,.T.);
#1510=FACE_OUTER_BOUND('',#2364,.T.);
#1511=FACE_OUTER_BOUND('',#2366,.T.);
#1512=FACE_OUTER_BOUND('',#2367,.T.);
#1513=FACE_OUTER_BOUND('',#2368,.T.);
#1514=FACE_OUTER_BOUND('',#2369,.T.);
#1515=FACE_OUTER_BOUND('',#2370,.T.);
#1516=FACE_OUTER_BOUND('',#2371,.T.);
#1517=FACE_OUTER_BOUND('',#2372,.T.);
#1518=FACE_OUTER_BOUND('',#2373,.T.);
#1519=FACE_OUTER_BOUND('',#2374,.T.);
#1520=FACE_OUTER_BOUND('',#2375,.T.);
#1521=FACE_OUTER_BOUND('',#2376,.T.);
#1522=FACE_OUTER_BOUND('',#2377,.T.);
#1523=FACE_OUTER_BOUND('',#2378,.T.);
#1524=FACE_OUTER_BOUND('',#2379,.T.);
#1525=FACE_OUTER_BOUND('',#2380,.T.);
#1526=FACE_OUTER_BOUND('',#2381,.T.);
#1527=FACE_OUTER_BOUND('',#2383,.T.);
#1528=FACE_OUTER_BOUND('',#2384,.T.);
#1529=FACE_OUTER_BOUND('',#2385,.T.);
#1530=FACE_OUTER_BOUND('',#2387,.T.);
#1531=FACE_OUTER_BOUND('',#2388,.T.);
#1532=FACE_OUTER_BOUND('',#2390,.T.);
#1533=FACE_OUTER_BOUND('',#2391,.T.);
#1534=FACE_OUTER_BOUND('',#2392,.T.);
#1535=FACE_OUTER_BOUND('',#2393,.T.);
#1536=FACE_OUTER_BOUND('',#2394,.T.);
#1537=FACE_OUTER_BOUND('',#2395,.T.);
#1538=FACE_OUTER_BOUND('',#2396,.T.);
#1539=FACE_OUTER_BOUND('',#2397,.T.);
#1540=FACE_OUTER_BOUND('',#2398,.T.);
#1541=FACE_OUTER_BOUND('',#2399,.T.);
#1542=FACE_OUTER_BOUND('',#2400,.T.);
#1543=FACE_OUTER_BOUND('',#2402,.T.);
#1544=FACE_OUTER_BOUND('',#2403,.T.);
#1545=FACE_OUTER_BOUND('',#2404,.T.);
#1546=FACE_OUTER_BOUND('',#2405,.T.);
#1547=FACE_OUTER_BOUND('',#2406,.T.);
#1548=FACE_OUTER_BOUND('',#2407,.T.);
#1549=FACE_OUTER_BOUND('',#2408,.T.);
#1550=FACE_OUTER_BOUND('',#2409,.T.);
#1551=FACE_OUTER_BOUND('',#2410,.T.);
#1552=FACE_OUTER_BOUND('',#2411,.T.);
#1553=FACE_OUTER_BOUND('',#2412,.T.);
#1554=FACE_OUTER_BOUND('',#2413,.T.);
#1555=FACE_OUTER_BOUND('',#2414,.T.);
#1556=FACE_OUTER_BOUND('',#2416,.T.);
#1557=FACE_OUTER_BOUND('',#2417,.T.);
#1558=FACE_OUTER_BOUND('',#2418,.T.);
#1559=FACE_OUTER_BOUND('',#2419,.T.);
#1560=FACE_OUTER_BOUND('',#2420,.T.);
#1561=FACE_OUTER_BOUND('',#2421,.T.);
#1562=FACE_OUTER_BOUND('',#2422,.T.);
#1563=FACE_OUTER_BOUND('',#2423,.T.);
#1564=FACE_OUTER_BOUND('',#2424,.T.);
#1565=FACE_OUTER_BOUND('',#2425,.T.);
#1566=FACE_OUTER_BOUND('',#2426,.T.);
#1567=FACE_OUTER_BOUND('',#2427,.T.);
#1568=FACE_OUTER_BOUND('',#2428,.T.);
#1569=FACE_OUTER_BOUND('',#2429,.T.);
#1570=FACE_OUTER_BOUND('',#2430,.T.);
#1571=FACE_OUTER_BOUND('',#2431,.T.);
#1572=FACE_OUTER_BOUND('',#2432,.T.);
#1573=FACE_OUTER_BOUND('',#2433,.T.);
#1574=FACE_OUTER_BOUND('',#2434,.T.);
#1575=FACE_OUTER_BOUND('',#2435,.T.);
#1576=FACE_OUTER_BOUND('',#2436,.T.);
#1577=FACE_OUTER_BOUND('',#2437,.T.);
#1578=FACE_OUTER_BOUND('',#2438,.T.);
#1579=FACE_OUTER_BOUND('',#2439,.T.);
#1580=FACE_OUTER_BOUND('',#2440,.T.);
#1581=FACE_OUTER_BOUND('',#2441,.T.);
#1582=FACE_OUTER_BOUND('',#2442,.T.);
#1583=FACE_OUTER_BOUND('',#2443,.T.);
#1584=FACE_OUTER_BOUND('',#2444,.T.);
#1585=FACE_OUTER_BOUND('',#2445,.T.);
#1586=FACE_OUTER_BOUND('',#2447,.T.);
#1587=FACE_OUTER_BOUND('',#2448,.T.);
#1588=FACE_OUTER_BOUND('',#2449,.T.);
#1589=FACE_OUTER_BOUND('',#2450,.T.);
#1590=FACE_OUTER_BOUND('',#2451,.T.);
#1591=FACE_OUTER_BOUND('',#2452,.T.);
#1592=FACE_OUTER_BOUND('',#2453,.T.);
#1593=FACE_OUTER_BOUND('',#2454,.T.);
#1594=FACE_OUTER_BOUND('',#2455,.T.);
#1595=FACE_OUTER_BOUND('',#2456,.T.);
#1596=FACE_OUTER_BOUND('',#2458,.T.);
#1597=FACE_OUTER_BOUND('',#2459,.T.);
#1598=FACE_OUTER_BOUND('',#2460,.T.);
#1599=FACE_OUTER_BOUND('',#2461,.T.);
#1600=FACE_OUTER_BOUND('',#2462,.T.);
#1601=FACE_OUTER_BOUND('',#2463,.T.);
#1602=FACE_OUTER_BOUND('',#2464,.T.);
#1603=FACE_OUTER_BOUND('',#2465,.T.);
#1604=FACE_OUTER_BOUND('',#2466,.T.);
#1605=FACE_OUTER_BOUND('',#2467,.T.);
#1606=FACE_OUTER_BOUND('',#2468,.T.);
#1607=FACE_OUTER_BOUND('',#2469,.T.);
#1608=FACE_OUTER_BOUND('',#2470,.T.);
#1609=FACE_OUTER_BOUND('',#2471,.T.);
#1610=FACE_OUTER_BOUND('',#2472,.T.);
#1611=FACE_OUTER_BOUND('',#2473,.T.);
#1612=FACE_OUTER_BOUND('',#2474,.T.);
#1613=FACE_OUTER_BOUND('',#2475,.T.);
#1614=FACE_OUTER_BOUND('',#2476,.T.);
#1615=FACE_OUTER_BOUND('',#2477,.T.);
#1616=FACE_OUTER_BOUND('',#2478,.T.);
#1617=FACE_OUTER_BOUND('',#2479,.T.);
#1618=FACE_OUTER_BOUND('',#2480,.T.);
#1619=FACE_OUTER_BOUND('',#2481,.T.);
#1620=FACE_OUTER_BOUND('',#2482,.T.);
#1621=FACE_OUTER_BOUND('',#2483,.T.);
#1622=FACE_OUTER_BOUND('',#2486,.T.);
#1623=FACE_OUTER_BOUND('',#2487,.T.);
#1624=FACE_OUTER_BOUND('',#2488,.T.);
#1625=FACE_OUTER_BOUND('',#2489,.T.);
#1626=FACE_OUTER_BOUND('',#2490,.T.);
#1627=FACE_OUTER_BOUND('',#2491,.T.);
#1628=FACE_OUTER_BOUND('',#2492,.T.);
#1629=FACE_OUTER_BOUND('',#2493,.T.);
#1630=FACE_OUTER_BOUND('',#2494,.T.);
#1631=FACE_OUTER_BOUND('',#2495,.T.);
#1632=FACE_OUTER_BOUND('',#2496,.T.);
#1633=FACE_OUTER_BOUND('',#2497,.T.);
#1634=FACE_OUTER_BOUND('',#2498,.T.);
#1635=FACE_OUTER_BOUND('',#2499,.T.);
#1636=FACE_OUTER_BOUND('',#2500,.T.);
#1637=FACE_OUTER_BOUND('',#2501,.T.);
#1638=FACE_OUTER_BOUND('',#2503,.T.);
#1639=FACE_OUTER_BOUND('',#2504,.T.);
#1640=FACE_OUTER_BOUND('',#2505,.T.);
#1641=FACE_OUTER_BOUND('',#2506,.T.);
#1642=FACE_OUTER_BOUND('',#2507,.T.);
#1643=FACE_OUTER_BOUND('',#2508,.T.);
#1644=FACE_OUTER_BOUND('',#2509,.T.);
#1645=FACE_OUTER_BOUND('',#2510,.T.);
#1646=FACE_OUTER_BOUND('',#2511,.T.);
#1647=FACE_OUTER_BOUND('',#2512,.T.);
#1648=FACE_OUTER_BOUND('',#2513,.T.);
#1649=FACE_OUTER_BOUND('',#2514,.T.);
#1650=FACE_OUTER_BOUND('',#2515,.T.);
#1651=FACE_OUTER_BOUND('',#2516,.T.);
#1652=FACE_OUTER_BOUND('',#2520,.T.);
#1653=FACE_OUTER_BOUND('',#2521,.T.);
#1654=FACE_OUTER_BOUND('',#2525,.T.);
#1655=FACE_OUTER_BOUND('',#2526,.T.);
#1656=FACE_OUTER_BOUND('',#2527,.T.);
#1657=FACE_OUTER_BOUND('',#2528,.T.);
#1658=FACE_OUTER_BOUND('',#2529,.T.);
#1659=FACE_OUTER_BOUND('',#2530,.T.);
#1660=FACE_OUTER_BOUND('',#2531,.T.);
#1661=FACE_OUTER_BOUND('',#2532,.T.);
#1662=FACE_OUTER_BOUND('',#2533,.T.);
#1663=FACE_OUTER_BOUND('',#2534,.T.);
#1664=FACE_OUTER_BOUND('',#2535,.T.);
#1665=FACE_OUTER_BOUND('',#2536,.T.);
#1666=FACE_OUTER_BOUND('',#2537,.T.);
#1667=FACE_OUTER_BOUND('',#2538,.T.);
#1668=FACE_OUTER_BOUND('',#2539,.T.);
#1669=FACE_OUTER_BOUND('',#2540,.T.);
#1670=FACE_OUTER_BOUND('',#2541,.T.);
#1671=FACE_OUTER_BOUND('',#2542,.T.);
#1672=FACE_OUTER_BOUND('',#2543,.T.);
#1673=FACE_OUTER_BOUND('',#2544,.T.);
#1674=FACE_OUTER_BOUND('',#2545,.T.);
#1675=FACE_OUTER_BOUND('',#2546,.T.);
#1676=FACE_OUTER_BOUND('',#2547,.T.);
#1677=FACE_OUTER_BOUND('',#2548,.T.);
#1678=FACE_OUTER_BOUND('',#2549,.T.);
#1679=FACE_OUTER_BOUND('',#2550,.T.);
#1680=FACE_OUTER_BOUND('',#2551,.T.);
#1681=FACE_OUTER_BOUND('',#2552,.T.);
#1682=FACE_OUTER_BOUND('',#2553,.T.);
#1683=FACE_OUTER_BOUND('',#2554,.T.);
#1684=FACE_OUTER_BOUND('',#2555,.T.);
#1685=FACE_OUTER_BOUND('',#2556,.T.);
#1686=FACE_OUTER_BOUND('',#2557,.T.);
#1687=FACE_OUTER_BOUND('',#2558,.T.);
#1688=FACE_OUTER_BOUND('',#2559,.T.);
#1689=FACE_OUTER_BOUND('',#2560,.T.);
#1690=FACE_OUTER_BOUND('',#2561,.T.);
#1691=FACE_OUTER_BOUND('',#2562,.T.);
#1692=FACE_OUTER_BOUND('',#2563,.T.);
#1693=FACE_OUTER_BOUND('',#2564,.T.);
#1694=FACE_OUTER_BOUND('',#2565,.T.);
#1695=FACE_OUTER_BOUND('',#2566,.T.);
#1696=FACE_OUTER_BOUND('',#2567,.T.);
#1697=FACE_OUTER_BOUND('',#2568,.T.);
#1698=FACE_OUTER_BOUND('',#2569,.T.);
#1699=FACE_OUTER_BOUND('',#2570,.T.);
#1700=FACE_OUTER_BOUND('',#2571,.T.);
#1701=FACE_OUTER_BOUND('',#2572,.T.);
#1702=FACE_OUTER_BOUND('',#2573,.T.);
#1703=FACE_OUTER_BOUND('',#2574,.T.);
#1704=FACE_OUTER_BOUND('',#2575,.T.);
#1705=FACE_OUTER_BOUND('',#2576,.T.);
#1706=FACE_OUTER_BOUND('',#2577,.T.);
#1707=FACE_OUTER_BOUND('',#2578,.T.);
#1708=FACE_OUTER_BOUND('',#2579,.T.);
#1709=FACE_OUTER_BOUND('',#2580,.T.);
#1710=FACE_OUTER_BOUND('',#2581,.T.);
#1711=FACE_OUTER_BOUND('',#2582,.T.);
#1712=FACE_OUTER_BOUND('',#2583,.T.);
#1713=FACE_OUTER_BOUND('',#2584,.T.);
#1714=FACE_OUTER_BOUND('',#2585,.T.);
#1715=FACE_OUTER_BOUND('',#2586,.T.);
#1716=FACE_OUTER_BOUND('',#2590,.T.);
#1717=FACE_OUTER_BOUND('',#2591,.T.);
#1718=FACE_OUTER_BOUND('',#2592,.T.);
#1719=FACE_OUTER_BOUND('',#2593,.T.);
#1720=FACE_OUTER_BOUND('',#2594,.T.);
#1721=FACE_OUTER_BOUND('',#2595,.T.);
#1722=FACE_OUTER_BOUND('',#2596,.T.);
#1723=FACE_OUTER_BOUND('',#2597,.T.);
#1724=FACE_OUTER_BOUND('',#2598,.T.);
#1725=FACE_OUTER_BOUND('',#2599,.T.);
#1726=FACE_OUTER_BOUND('',#2600,.T.);
#1727=FACE_OUTER_BOUND('',#2601,.T.);
#1728=FACE_OUTER_BOUND('',#2602,.T.);
#1729=FACE_OUTER_BOUND('',#2603,.T.);
#1730=FACE_OUTER_BOUND('',#2604,.T.);
#1731=FACE_OUTER_BOUND('',#2605,.T.);
#1732=FACE_OUTER_BOUND('',#2606,.T.);
#1733=FACE_OUTER_BOUND('',#2607,.T.);
#1734=FACE_OUTER_BOUND('',#2608,.T.);
#1735=FACE_OUTER_BOUND('',#2609,.T.);
#1736=FACE_OUTER_BOUND('',#2610,.T.);
#1737=FACE_OUTER_BOUND('',#2611,.T.);
#1738=FACE_OUTER_BOUND('',#2612,.T.);
#1739=FACE_OUTER_BOUND('',#2613,.T.);
#1740=FACE_OUTER_BOUND('',#2615,.T.);
#1741=FACE_OUTER_BOUND('',#2616,.T.);
#1742=FACE_OUTER_BOUND('',#2618,.T.);
#1743=FACE_OUTER_BOUND('',#2619,.T.);
#1744=FACE_OUTER_BOUND('',#2620,.T.);
#1745=FACE_OUTER_BOUND('',#2621,.T.);
#1746=FACE_OUTER_BOUND('',#2622,.T.);
#1747=FACE_OUTER_BOUND('',#2623,.T.);
#1748=FACE_OUTER_BOUND('',#2624,.T.);
#1749=FACE_OUTER_BOUND('',#2625,.T.);
#1750=FACE_OUTER_BOUND('',#2626,.T.);
#1751=FACE_OUTER_BOUND('',#2627,.T.);
#1752=FACE_OUTER_BOUND('',#2628,.T.);
#1753=FACE_OUTER_BOUND('',#2629,.T.);
#1754=FACE_OUTER_BOUND('',#2630,.T.);
#1755=FACE_OUTER_BOUND('',#2631,.T.);
#1756=FACE_OUTER_BOUND('',#2632,.T.);
#1757=FACE_OUTER_BOUND('',#2633,.T.);
#1758=FACE_OUTER_BOUND('',#2634,.T.);
#1759=FACE_OUTER_BOUND('',#2635,.T.);
#1760=FACE_OUTER_BOUND('',#2636,.T.);
#1761=FACE_OUTER_BOUND('',#2637,.T.);
#1762=FACE_OUTER_BOUND('',#2638,.T.);
#1763=FACE_OUTER_BOUND('',#2639,.T.);
#1764=FACE_OUTER_BOUND('',#2640,.T.);
#1765=FACE_OUTER_BOUND('',#2641,.T.);
#1766=FACE_OUTER_BOUND('',#2642,.T.);
#1767=FACE_OUTER_BOUND('',#2643,.T.);
#1768=FACE_OUTER_BOUND('',#2644,.T.);
#1769=FACE_OUTER_BOUND('',#2645,.T.);
#1770=FACE_OUTER_BOUND('',#2646,.T.);
#1771=FACE_OUTER_BOUND('',#2647,.T.);
#1772=FACE_OUTER_BOUND('',#2648,.T.);
#1773=FACE_OUTER_BOUND('',#2649,.T.);
#1774=FACE_OUTER_BOUND('',#2650,.T.);
#1775=FACE_OUTER_BOUND('',#2651,.T.);
#1776=FACE_OUTER_BOUND('',#2652,.T.);
#1777=FACE_OUTER_BOUND('',#2653,.T.);
#1778=FACE_OUTER_BOUND('',#2654,.T.);
#1779=FACE_OUTER_BOUND('',#2655,.T.);
#1780=FACE_OUTER_BOUND('',#2656,.T.);
#1781=FACE_OUTER_BOUND('',#2657,.T.);
#1782=FACE_OUTER_BOUND('',#2658,.T.);
#1783=FACE_OUTER_BOUND('',#2659,.T.);
#1784=FACE_OUTER_BOUND('',#2660,.T.);
#1785=FACE_OUTER_BOUND('',#2661,.T.);
#1786=FACE_OUTER_BOUND('',#2662,.T.);
#1787=FACE_OUTER_BOUND('',#2663,.T.);
#1788=FACE_OUTER_BOUND('',#2664,.T.);
#1789=FACE_OUTER_BOUND('',#2665,.T.);
#1790=FACE_OUTER_BOUND('',#2666,.T.);
#1791=FACE_OUTER_BOUND('',#2667,.T.);
#1792=FACE_OUTER_BOUND('',#2668,.T.);
#1793=FACE_OUTER_BOUND('',#2669,.T.);
#1794=FACE_OUTER_BOUND('',#2670,.T.);
#1795=FACE_OUTER_BOUND('',#2671,.T.);
#1796=FACE_OUTER_BOUND('',#2672,.T.);
#1797=FACE_OUTER_BOUND('',#2673,.T.);
#1798=FACE_OUTER_BOUND('',#2674,.T.);
#1799=FACE_OUTER_BOUND('',#2675,.T.);
#1800=FACE_OUTER_BOUND('',#2676,.T.);
#1801=FACE_OUTER_BOUND('',#2677,.T.);
#1802=FACE_OUTER_BOUND('',#2679,.T.);
#1803=FACE_OUTER_BOUND('',#2680,.T.);
#1804=FACE_OUTER_BOUND('',#2681,.T.);
#1805=FACE_OUTER_BOUND('',#2682,.T.);
#1806=FACE_OUTER_BOUND('',#2683,.T.);
#1807=FACE_OUTER_BOUND('',#2684,.T.);
#1808=FACE_OUTER_BOUND('',#2685,.T.);
#1809=FACE_OUTER_BOUND('',#2686,.T.);
#1810=FACE_OUTER_BOUND('',#2687,.T.);
#1811=FACE_OUTER_BOUND('',#2688,.T.);
#1812=FACE_OUTER_BOUND('',#2689,.T.);
#1813=FACE_OUTER_BOUND('',#2690,.T.);
#1814=FACE_OUTER_BOUND('',#2691,.T.);
#1815=FACE_OUTER_BOUND('',#2692,.T.);
#1816=FACE_OUTER_BOUND('',#2693,.T.);
#1817=FACE_OUTER_BOUND('',#2694,.T.);
#1818=FACE_OUTER_BOUND('',#2695,.T.);
#1819=FACE_OUTER_BOUND('',#2696,.T.);
#1820=FACE_OUTER_BOUND('',#2697,.T.);
#1821=FACE_OUTER_BOUND('',#2698,.T.);
#1822=FACE_OUTER_BOUND('',#2699,.T.);
#1823=FACE_OUTER_BOUND('',#2700,.T.);
#1824=FACE_OUTER_BOUND('',#2701,.T.);
#1825=FACE_OUTER_BOUND('',#2702,.T.);
#1826=FACE_OUTER_BOUND('',#2703,.T.);
#1827=FACE_OUTER_BOUND('',#2704,.T.);
#1828=FACE_OUTER_BOUND('',#2705,.T.);
#1829=FACE_OUTER_BOUND('',#2706,.T.);
#1830=FACE_OUTER_BOUND('',#2707,.T.);
#1831=FACE_OUTER_BOUND('',#2708,.T.);
#1832=FACE_OUTER_BOUND('',#2709,.T.);
#1833=FACE_OUTER_BOUND('',#2710,.T.);
#1834=FACE_OUTER_BOUND('',#2711,.T.);
#1835=FACE_OUTER_BOUND('',#2712,.T.);
#1836=FACE_OUTER_BOUND('',#2713,.T.);
#1837=FACE_OUTER_BOUND('',#2714,.T.);
#1838=FACE_OUTER_BOUND('',#2715,.T.);
#1839=FACE_OUTER_BOUND('',#2716,.T.);
#1840=FACE_OUTER_BOUND('',#2717,.T.);
#1841=FACE_OUTER_BOUND('',#2718,.T.);
#1842=FACE_OUTER_BOUND('',#2719,.T.);
#1843=FACE_OUTER_BOUND('',#2720,.T.);
#1844=FACE_OUTER_BOUND('',#2721,.T.);
#1845=FACE_OUTER_BOUND('',#2722,.T.);
#1846=FACE_OUTER_BOUND('',#2723,.T.);
#1847=FACE_OUTER_BOUND('',#2724,.T.);
#1848=FACE_OUTER_BOUND('',#2725,.T.);
#1849=FACE_OUTER_BOUND('',#2726,.T.);
#1850=FACE_OUTER_BOUND('',#2727,.T.);
#1851=FACE_OUTER_BOUND('',#2728,.T.);
#1852=FACE_OUTER_BOUND('',#2729,.T.);
#1853=FACE_OUTER_BOUND('',#2730,.T.);
#1854=FACE_OUTER_BOUND('',#2731,.T.);
#1855=FACE_OUTER_BOUND('',#2732,.T.);
#1856=FACE_OUTER_BOUND('',#2733,.T.);
#1857=FACE_OUTER_BOUND('',#2734,.T.);
#1858=FACE_OUTER_BOUND('',#2735,.T.);
#1859=FACE_OUTER_BOUND('',#2736,.T.);
#1860=FACE_OUTER_BOUND('',#2737,.T.);
#1861=FACE_OUTER_BOUND('',#2738,.T.);
#1862=FACE_OUTER_BOUND('',#2739,.T.);
#1863=FACE_OUTER_BOUND('',#2740,.T.);
#1864=FACE_OUTER_BOUND('',#2741,.T.);
#1865=FACE_OUTER_BOUND('',#2742,.T.);
#1866=FACE_OUTER_BOUND('',#2743,.T.);
#1867=FACE_OUTER_BOUND('',#2744,.T.);
#1868=FACE_OUTER_BOUND('',#2745,.T.);
#1869=FACE_OUTER_BOUND('',#2746,.T.);
#1870=FACE_OUTER_BOUND('',#2747,.T.);
#1871=FACE_OUTER_BOUND('',#2748,.T.);
#1872=FACE_OUTER_BOUND('',#2749,.T.);
#1873=FACE_OUTER_BOUND('',#2750,.T.);
#1874=FACE_OUTER_BOUND('',#2751,.T.);
#1875=FACE_OUTER_BOUND('',#2752,.T.);
#1876=FACE_OUTER_BOUND('',#2753,.T.);
#1877=FACE_OUTER_BOUND('',#2754,.T.);
#1878=FACE_OUTER_BOUND('',#2755,.T.);
#1879=FACE_OUTER_BOUND('',#2756,.T.);
#1880=FACE_OUTER_BOUND('',#2757,.T.);
#1881=FACE_OUTER_BOUND('',#2758,.T.);
#1882=FACE_OUTER_BOUND('',#2759,.T.);
#1883=FACE_OUTER_BOUND('',#2760,.T.);
#1884=FACE_OUTER_BOUND('',#2761,.T.);
#1885=FACE_OUTER_BOUND('',#2762,.T.);
#1886=FACE_OUTER_BOUND('',#2763,.T.);
#1887=FACE_OUTER_BOUND('',#2764,.T.);
#1888=FACE_OUTER_BOUND('',#2765,.T.);
#1889=FACE_OUTER_BOUND('',#2766,.T.);
#1890=FACE_OUTER_BOUND('',#2767,.T.);
#1891=FACE_OUTER_BOUND('',#2768,.T.);
#1892=FACE_OUTER_BOUND('',#2769,.T.);
#1893=FACE_OUTER_BOUND('',#2770,.T.);
#1894=FACE_OUTER_BOUND('',#2771,.T.);
#1895=FACE_OUTER_BOUND('',#2772,.T.);
#1896=FACE_OUTER_BOUND('',#2773,.T.);
#1897=FACE_OUTER_BOUND('',#2774,.T.);
#1898=FACE_OUTER_BOUND('',#2775,.T.);
#1899=FACE_OUTER_BOUND('',#2776,.T.);
#1900=FACE_OUTER_BOUND('',#2777,.T.);
#1901=FACE_OUTER_BOUND('',#2778,.T.);
#1902=FACE_OUTER_BOUND('',#2779,.T.);
#1903=FACE_OUTER_BOUND('',#2780,.T.);
#1904=FACE_OUTER_BOUND('',#2781,.T.);
#1905=FACE_OUTER_BOUND('',#2782,.T.);
#1906=FACE_OUTER_BOUND('',#2783,.T.);
#1907=FACE_OUTER_BOUND('',#2785,.T.);
#1908=FACE_OUTER_BOUND('',#2786,.T.);
#1909=FACE_OUTER_BOUND('',#2787,.T.);
#1910=FACE_OUTER_BOUND('',#2788,.T.);
#1911=FACE_OUTER_BOUND('',#2789,.T.);
#1912=FACE_OUTER_BOUND('',#2791,.T.);
#1913=FACE_OUTER_BOUND('',#2792,.T.);
#1914=FACE_OUTER_BOUND('',#2793,.T.);
#1915=FACE_OUTER_BOUND('',#2794,.T.);
#1916=FACE_OUTER_BOUND('',#2795,.T.);
#1917=FACE_OUTER_BOUND('',#2796,.T.);
#1918=FACE_OUTER_BOUND('',#2797,.T.);
#1919=FACE_OUTER_BOUND('',#2798,.T.);
#1920=FACE_OUTER_BOUND('',#2799,.T.);
#1921=FACE_OUTER_BOUND('',#2800,.T.);
#1922=FACE_OUTER_BOUND('',#2801,.T.);
#1923=FACE_OUTER_BOUND('',#2802,.T.);
#1924=FACE_OUTER_BOUND('',#2803,.T.);
#1925=FACE_OUTER_BOUND('',#2804,.T.);
#1926=FACE_OUTER_BOUND('',#2805,.T.);
#1927=FACE_OUTER_BOUND('',#2806,.T.);
#1928=FACE_OUTER_BOUND('',#2807,.T.);
#1929=FACE_OUTER_BOUND('',#2808,.T.);
#1930=FACE_OUTER_BOUND('',#2809,.T.);
#1931=FACE_OUTER_BOUND('',#2810,.T.);
#1932=FACE_OUTER_BOUND('',#2811,.T.);
#1933=FACE_OUTER_BOUND('',#2812,.T.);
#1934=FACE_OUTER_BOUND('',#2813,.T.);
#1935=FACE_OUTER_BOUND('',#2814,.T.);
#1936=FACE_OUTER_BOUND('',#2815,.T.);
#1937=FACE_OUTER_BOUND('',#2816,.T.);
#1938=FACE_OUTER_BOUND('',#2817,.T.);
#1939=FACE_OUTER_BOUND('',#2818,.T.);
#1940=FACE_OUTER_BOUND('',#2819,.T.);
#1941=FACE_OUTER_BOUND('',#2820,.T.);
#1942=FACE_OUTER_BOUND('',#2821,.T.);
#1943=FACE_OUTER_BOUND('',#2822,.T.);
#1944=FACE_OUTER_BOUND('',#2823,.T.);
#1945=FACE_OUTER_BOUND('',#2824,.T.);
#1946=FACE_OUTER_BOUND('',#2825,.T.);
#1947=FACE_OUTER_BOUND('',#2826,.T.);
#1948=FACE_OUTER_BOUND('',#2827,.T.);
#1949=FACE_OUTER_BOUND('',#2828,.T.);
#1950=FACE_OUTER_BOUND('',#2830,.T.);
#1951=FACE_OUTER_BOUND('',#2831,.T.);
#1952=FACE_OUTER_BOUND('',#2832,.T.);
#1953=FACE_OUTER_BOUND('',#2833,.T.);
#1954=FACE_OUTER_BOUND('',#2834,.T.);
#1955=FACE_OUTER_BOUND('',#2835,.T.);
#1956=FACE_OUTER_BOUND('',#2836,.T.);
#1957=FACE_OUTER_BOUND('',#2837,.T.);
#1958=FACE_OUTER_BOUND('',#2838,.T.);
#1959=FACE_OUTER_BOUND('',#2839,.T.);
#1960=FACE_OUTER_BOUND('',#2841,.T.);
#1961=FACE_OUTER_BOUND('',#2842,.T.);
#1962=FACE_OUTER_BOUND('',#2843,.T.);
#1963=FACE_OUTER_BOUND('',#2844,.T.);
#1964=FACE_OUTER_BOUND('',#2845,.T.);
#1965=FACE_OUTER_BOUND('',#2846,.T.);
#1966=FACE_OUTER_BOUND('',#2847,.T.);
#1967=FACE_OUTER_BOUND('',#2848,.T.);
#1968=FACE_OUTER_BOUND('',#2849,.T.);
#1969=FACE_OUTER_BOUND('',#2850,.T.);
#1970=FACE_OUTER_BOUND('',#2851,.T.);
#1971=FACE_OUTER_BOUND('',#2852,.T.);
#1972=FACE_OUTER_BOUND('',#2853,.T.);
#1973=FACE_OUTER_BOUND('',#2854,.T.);
#1974=FACE_OUTER_BOUND('',#2855,.T.);
#1975=FACE_OUTER_BOUND('',#2856,.T.);
#1976=FACE_OUTER_BOUND('',#2857,.T.);
#1977=FACE_OUTER_BOUND('',#2858,.T.);
#1978=FACE_OUTER_BOUND('',#2859,.T.);
#1979=FACE_OUTER_BOUND('',#2860,.T.);
#1980=FACE_OUTER_BOUND('',#2861,.T.);
#1981=FACE_OUTER_BOUND('',#2862,.T.);
#1982=FACE_OUTER_BOUND('',#2863,.T.);
#1983=FACE_OUTER_BOUND('',#2864,.T.);
#1984=FACE_OUTER_BOUND('',#2865,.T.);
#1985=FACE_OUTER_BOUND('',#2866,.T.);
#1986=FACE_OUTER_BOUND('',#2867,.T.);
#1987=FACE_OUTER_BOUND('',#2868,.T.);
#1988=FACE_OUTER_BOUND('',#2869,.T.);
#1989=FACE_OUTER_BOUND('',#2870,.T.);
#1990=FACE_OUTER_BOUND('',#2871,.T.);
#1991=FACE_OUTER_BOUND('',#2872,.T.);
#1992=FACE_OUTER_BOUND('',#2873,.T.);
#1993=FACE_OUTER_BOUND('',#2874,.T.);
#1994=FACE_OUTER_BOUND('',#2875,.T.);
#1995=FACE_OUTER_BOUND('',#2876,.T.);
#1996=FACE_OUTER_BOUND('',#2877,.T.);
#1997=FACE_OUTER_BOUND('',#2878,.T.);
#1998=FACE_OUTER_BOUND('',#2879,.T.);
#1999=FACE_OUTER_BOUND('',#2880,.T.);
#2000=FACE_OUTER_BOUND('',#2881,.T.);
#2001=FACE_OUTER_BOUND('',#2882,.T.);
#2002=FACE_OUTER_BOUND('',#2883,.T.);
#2003=FACE_OUTER_BOUND('',#2884,.T.);
#2004=FACE_OUTER_BOUND('',#2885,.T.);
#2005=FACE_OUTER_BOUND('',#2886,.T.);
#2006=FACE_OUTER_BOUND('',#2887,.T.);
#2007=FACE_OUTER_BOUND('',#2888,.T.);
#2008=FACE_OUTER_BOUND('',#2889,.T.);
#2009=FACE_OUTER_BOUND('',#2890,.T.);
#2010=FACE_OUTER_BOUND('',#2891,.T.);
#2011=FACE_OUTER_BOUND('',#2892,.T.);
#2012=FACE_OUTER_BOUND('',#2893,.T.);
#2013=FACE_OUTER_BOUND('',#2894,.T.);
#2014=FACE_OUTER_BOUND('',#2895,.T.);
#2015=FACE_OUTER_BOUND('',#2896,.T.);
#2016=FACE_OUTER_BOUND('',#2897,.T.);
#2017=FACE_OUTER_BOUND('',#2898,.T.);
#2018=FACE_OUTER_BOUND('',#2899,.T.);
#2019=FACE_OUTER_BOUND('',#2900,.T.);
#2020=FACE_OUTER_BOUND('',#2901,.T.);
#2021=FACE_OUTER_BOUND('',#2902,.T.);
#2022=FACE_OUTER_BOUND('',#2903,.T.);
#2023=FACE_OUTER_BOUND('',#2904,.T.);
#2024=FACE_OUTER_BOUND('',#2905,.T.);
#2025=FACE_OUTER_BOUND('',#2906,.T.);
#2026=FACE_OUTER_BOUND('',#2907,.T.);
#2027=FACE_OUTER_BOUND('',#2908,.T.);
#2028=FACE_OUTER_BOUND('',#2909,.T.);
#2029=FACE_OUTER_BOUND('',#2910,.T.);
#2030=FACE_OUTER_BOUND('',#2911,.T.);
#2031=FACE_OUTER_BOUND('',#2912,.T.);
#2032=FACE_OUTER_BOUND('',#2913,.T.);
#2033=FACE_OUTER_BOUND('',#2914,.T.);
#2034=FACE_OUTER_BOUND('',#2915,.T.);
#2035=FACE_OUTER_BOUND('',#2916,.T.);
#2036=FACE_OUTER_BOUND('',#2917,.T.);
#2037=FACE_OUTER_BOUND('',#2918,.T.);
#2038=FACE_OUTER_BOUND('',#2919,.T.);
#2039=FACE_OUTER_BOUND('',#2920,.T.);
#2040=FACE_OUTER_BOUND('',#2921,.T.);
#2041=FACE_OUTER_BOUND('',#2922,.T.);
#2042=FACE_OUTER_BOUND('',#2923,.T.);
#2043=FACE_OUTER_BOUND('',#2924,.T.);
#2044=FACE_OUTER_BOUND('',#2925,.T.);
#2045=FACE_OUTER_BOUND('',#2926,.T.);
#2046=FACE_OUTER_BOUND('',#2927,.T.);
#2047=FACE_OUTER_BOUND('',#2928,.T.);
#2048=FACE_OUTER_BOUND('',#2929,.T.);
#2049=FACE_OUTER_BOUND('',#2930,.T.);
#2050=FACE_OUTER_BOUND('',#2931,.T.);
#2051=FACE_OUTER_BOUND('',#2932,.T.);
#2052=FACE_OUTER_BOUND('',#2933,.T.);
#2053=FACE_OUTER_BOUND('',#2934,.T.);
#2054=FACE_OUTER_BOUND('',#2935,.T.);
#2055=FACE_OUTER_BOUND('',#2936,.T.);
#2056=FACE_OUTER_BOUND('',#2938,.T.);
#2057=FACE_OUTER_BOUND('',#2939,.T.);
#2058=FACE_OUTER_BOUND('',#2940,.T.);
#2059=FACE_OUTER_BOUND('',#2941,.T.);
#2060=FACE_OUTER_BOUND('',#2942,.T.);
#2061=FACE_OUTER_BOUND('',#2943,.T.);
#2062=FACE_OUTER_BOUND('',#2944,.T.);
#2063=FACE_OUTER_BOUND('',#2945,.T.);
#2064=FACE_OUTER_BOUND('',#2946,.T.);
#2065=FACE_OUTER_BOUND('',#2947,.T.);
#2066=FACE_OUTER_BOUND('',#2948,.T.);
#2067=FACE_OUTER_BOUND('',#2949,.T.);
#2068=FACE_OUTER_BOUND('',#2950,.T.);
#2069=FACE_OUTER_BOUND('',#2951,.T.);
#2070=FACE_OUTER_BOUND('',#2952,.T.);
#2071=FACE_OUTER_BOUND('',#2953,.T.);
#2072=FACE_OUTER_BOUND('',#2954,.T.);
#2073=FACE_OUTER_BOUND('',#2955,.T.);
#2074=FACE_OUTER_BOUND('',#2956,.T.);
#2075=FACE_OUTER_BOUND('',#2957,.T.);
#2076=FACE_OUTER_BOUND('',#2958,.T.);
#2077=FACE_OUTER_BOUND('',#2959,.T.);
#2078=FACE_OUTER_BOUND('',#2960,.T.);
#2079=FACE_OUTER_BOUND('',#2961,.T.);
#2080=FACE_OUTER_BOUND('',#2962,.T.);
#2081=FACE_OUTER_BOUND('',#2963,.T.);
#2082=FACE_OUTER_BOUND('',#2964,.T.);
#2083=FACE_OUTER_BOUND('',#2965,.T.);
#2084=FACE_OUTER_BOUND('',#2966,.T.);
#2085=FACE_OUTER_BOUND('',#2967,.T.);
#2086=FACE_OUTER_BOUND('',#2968,.T.);
#2087=FACE_OUTER_BOUND('',#2969,.T.);
#2088=FACE_OUTER_BOUND('',#2970,.T.);
#2089=FACE_OUTER_BOUND('',#2971,.T.);
#2090=FACE_OUTER_BOUND('',#2972,.T.);
#2091=FACE_OUTER_BOUND('',#2973,.T.);
#2092=FACE_OUTER_BOUND('',#2974,.T.);
#2093=FACE_OUTER_BOUND('',#2975,.T.);
#2094=FACE_OUTER_BOUND('',#2976,.T.);
#2095=FACE_OUTER_BOUND('',#2977,.T.);
#2096=FACE_OUTER_BOUND('',#2978,.T.);
#2097=FACE_OUTER_BOUND('',#2979,.T.);
#2098=FACE_OUTER_BOUND('',#2980,.T.);
#2099=FACE_OUTER_BOUND('',#2981,.T.);
#2100=FACE_OUTER_BOUND('',#2982,.T.);
#2101=FACE_OUTER_BOUND('',#2983,.T.);
#2102=FACE_OUTER_BOUND('',#2984,.T.);
#2103=FACE_OUTER_BOUND('',#2985,.T.);
#2104=FACE_OUTER_BOUND('',#2986,.T.);
#2105=FACE_OUTER_BOUND('',#2987,.T.);
#2106=FACE_OUTER_BOUND('',#2988,.T.);
#2107=FACE_OUTER_BOUND('',#2989,.T.);
#2108=FACE_OUTER_BOUND('',#2990,.T.);
#2109=FACE_OUTER_BOUND('',#2991,.T.);
#2110=FACE_OUTER_BOUND('',#2992,.T.);
#2111=FACE_OUTER_BOUND('',#2993,.T.);
#2112=FACE_OUTER_BOUND('',#2994,.T.);
#2113=FACE_OUTER_BOUND('',#2995,.T.);
#2114=FACE_OUTER_BOUND('',#2996,.T.);
#2115=FACE_OUTER_BOUND('',#2997,.T.);
#2116=FACE_OUTER_BOUND('',#2998,.T.);
#2117=FACE_OUTER_BOUND('',#2999,.T.);
#2118=FACE_OUTER_BOUND('',#3000,.T.);
#2119=FACE_OUTER_BOUND('',#3001,.T.);
#2120=FACE_OUTER_BOUND('',#3002,.T.);
#2121=FACE_OUTER_BOUND('',#3003,.T.);
#2122=FACE_OUTER_BOUND('',#3004,.T.);
#2123=FACE_OUTER_BOUND('',#3005,.T.);
#2124=FACE_OUTER_BOUND('',#3007,.T.);
#2125=FACE_OUTER_BOUND('',#3008,.T.);
#2126=FACE_OUTER_BOUND('',#3009,.T.);
#2127=FACE_OUTER_BOUND('',#3010,.T.);
#2128=FACE_OUTER_BOUND('',#3012,.T.);
#2129=FACE_OUTER_BOUND('',#3013,.T.);
#2130=FACE_OUTER_BOUND('',#3014,.T.);
#2131=FACE_OUTER_BOUND('',#3015,.T.);
#2132=FACE_OUTER_BOUND('',#3016,.T.);
#2133=FACE_OUTER_BOUND('',#3018,.T.);
#2134=FACE_OUTER_BOUND('',#3019,.T.);
#2135=FACE_OUTER_BOUND('',#3021,.T.);
#2136=FACE_OUTER_BOUND('',#3022,.T.);
#2137=FACE_OUTER_BOUND('',#3023,.T.);
#2138=FACE_OUTER_BOUND('',#3024,.T.);
#2139=FACE_OUTER_BOUND('',#3025,.T.);
#2140=FACE_OUTER_BOUND('',#3026,.T.);
#2141=FACE_OUTER_BOUND('',#3027,.T.);
#2142=FACE_OUTER_BOUND('',#3029,.T.);
#2143=FACE_OUTER_BOUND('',#3030,.T.);
#2144=FACE_OUTER_BOUND('',#3032,.T.);
#2145=FACE_OUTER_BOUND('',#3033,.T.);
#2146=FACE_OUTER_BOUND('',#3034,.T.);
#2147=FACE_OUTER_BOUND('',#3035,.T.);
#2148=FACE_OUTER_BOUND('',#3036,.T.);
#2149=FACE_OUTER_BOUND('',#3037,.T.);
#2150=FACE_OUTER_BOUND('',#3038,.T.);
#2151=FACE_OUTER_BOUND('',#3039,.T.);
#2152=FACE_OUTER_BOUND('',#3040,.T.);
#2153=FACE_OUTER_BOUND('',#3041,.T.);
#2154=FACE_OUTER_BOUND('',#3042,.T.);
#2155=FACE_OUTER_BOUND('',#3043,.T.);
#2156=FACE_OUTER_BOUND('',#3044,.T.);
#2157=FACE_OUTER_BOUND('',#3045,.T.);
#2158=FACE_OUTER_BOUND('',#3046,.T.);
#2159=FACE_OUTER_BOUND('',#3047,.T.);
#2160=FACE_OUTER_BOUND('',#3048,.T.);
#2161=FACE_OUTER_BOUND('',#3049,.T.);
#2162=FACE_OUTER_BOUND('',#3050,.T.);
#2163=FACE_OUTER_BOUND('',#3051,.T.);
#2164=FACE_OUTER_BOUND('',#3052,.T.);
#2165=FACE_OUTER_BOUND('',#3053,.T.);
#2166=FACE_OUTER_BOUND('',#3054,.T.);
#2167=FACE_OUTER_BOUND('',#3055,.T.);
#2168=FACE_OUTER_BOUND('',#3056,.T.);
#2169=FACE_OUTER_BOUND('',#3057,.T.);
#2170=FACE_OUTER_BOUND('',#3058,.T.);
#2171=FACE_OUTER_BOUND('',#3059,.T.);
#2172=FACE_OUTER_BOUND('',#3060,.T.);
#2173=FACE_OUTER_BOUND('',#3061,.T.);
#2174=FACE_OUTER_BOUND('',#3062,.T.);
#2175=FACE_OUTER_BOUND('',#3063,.T.);
#2176=FACE_OUTER_BOUND('',#3064,.T.);
#2177=FACE_OUTER_BOUND('',#3065,.T.);
#2178=FACE_OUTER_BOUND('',#3066,.T.);
#2179=FACE_OUTER_BOUND('',#3067,.T.);
#2180=FACE_OUTER_BOUND('',#3068,.T.);
#2181=FACE_OUTER_BOUND('',#3069,.T.);
#2182=FACE_OUTER_BOUND('',#3070,.T.);
#2183=FACE_OUTER_BOUND('',#3071,.T.);
#2184=FACE_OUTER_BOUND('',#3072,.T.);
#2185=FACE_OUTER_BOUND('',#3073,.T.);
#2186=FACE_OUTER_BOUND('',#3074,.T.);
#2187=FACE_OUTER_BOUND('',#3075,.T.);
#2188=FACE_OUTER_BOUND('',#3076,.T.);
#2189=FACE_OUTER_BOUND('',#3077,.T.);
#2190=FACE_OUTER_BOUND('',#3078,.T.);
#2191=FACE_OUTER_BOUND('',#3079,.T.);
#2192=FACE_OUTER_BOUND('',#3080,.T.);
#2193=FACE_OUTER_BOUND('',#3081,.T.);
#2194=FACE_OUTER_BOUND('',#3082,.T.);
#2195=FACE_OUTER_BOUND('',#3083,.T.);
#2196=FACE_OUTER_BOUND('',#3084,.T.);
#2197=FACE_OUTER_BOUND('',#3085,.T.);
#2198=FACE_OUTER_BOUND('',#3086,.T.);
#2199=FACE_OUTER_BOUND('',#3087,.T.);
#2200=FACE_OUTER_BOUND('',#3088,.T.);
#2201=FACE_OUTER_BOUND('',#3089,.T.);
#2202=FACE_OUTER_BOUND('',#3091,.T.);
#2203=FACE_OUTER_BOUND('',#3092,.T.);
#2204=FACE_OUTER_BOUND('',#3093,.T.);
#2205=FACE_OUTER_BOUND('',#3094,.T.);
#2206=FACE_OUTER_BOUND('',#3096,.T.);
#2207=FACE_OUTER_BOUND('',#3097,.T.);
#2208=EDGE_LOOP('',(#9171,#9172,#9173,#9174,#9175,#9176));
#2209=EDGE_LOOP('',(#9177,#9178,#9179,#9180,#9181));
#2210=EDGE_LOOP('',(#9182,#9183,#9184,#9185,#9186,#9187));
#2211=EDGE_LOOP('',(#9188,#9189,#9190,#9191));
#2212=EDGE_LOOP('',(#9192,#9193,#9194));
#2213=EDGE_LOOP('',(#9195,#9196,#9197));
#2214=EDGE_LOOP('',(#9198,#9199,#9200,#9201));
#2215=EDGE_LOOP('',(#9202,#9203,#9204,#9205));
#2216=EDGE_LOOP('',(#9206,#9207,#9208,#9209));
#2217=EDGE_LOOP('',(#9210,#9211,#9212,#9213,#9214));
#2218=EDGE_LOOP('',(#9215,#9216,#9217,#9218));
#2219=EDGE_LOOP('',(#9219,#9220,#9221,#9222));
#2220=EDGE_LOOP('',(#9223,#9224,#9225,#9226));
#2221=EDGE_LOOP('',(#9227,#9228,#9229,#9230));
#2222=EDGE_LOOP('',(#9231,#9232,#9233,#9234,#9235,#9236,#9237,#9238,#9239,
#9240));
#2223=EDGE_LOOP('',(#9241,#9242,#9243,#9244));
#2224=EDGE_LOOP('',(#9245,#9246,#9247,#9248));
#2225=EDGE_LOOP('',(#9249,#9250,#9251,#9252,#9253,#9254));
#2226=EDGE_LOOP('',(#9255));
#2227=EDGE_LOOP('',(#9256,#9257,#9258,#9259,#9260,#9261));
#2228=EDGE_LOOP('',(#9262,#9263,#9264,#9265,#9266));
#2229=EDGE_LOOP('',(#9267,#9268,#9269));
#2230=EDGE_LOOP('',(#9270,#9271,#9272));
#2231=EDGE_LOOP('',(#9273,#9274,#9275,#9276,#9277));
#2232=EDGE_LOOP('',(#9278,#9279,#9280,#9281));
#2233=EDGE_LOOP('',(#9282,#9283,#9284,#9285));
#2234=EDGE_LOOP('',(#9286,#9287,#9288,#9289));
#2235=EDGE_LOOP('',(#9290,#9291,#9292,#9293));
#2236=EDGE_LOOP('',(#9294,#9295,#9296,#9297));
#2237=EDGE_LOOP('',(#9298,#9299,#9300,#9301));
#2238=EDGE_LOOP('',(#9302,#9303,#9304,#9305));
#2239=EDGE_LOOP('',(#9306,#9307,#9308,#9309,#9310,#9311));
#2240=EDGE_LOOP('',(#9312,#9313,#9314,#9315));
#2241=EDGE_LOOP('',(#9316));
#2242=EDGE_LOOP('',(#9317,#9318,#9319,#9320,#9321,#9322));
#2243=EDGE_LOOP('',(#9323,#9324,#9325,#9326,#9327,#9328));
#2244=EDGE_LOOP('',(#9329,#9330,#9331,#9332));
#2245=EDGE_LOOP('',(#9333,#9334,#9335,#9336));
#2246=EDGE_LOOP('',(#9337,#9338,#9339,#9340));
#2247=EDGE_LOOP('',(#9341,#9342,#9343,#9344,#9345,#9346,#9347,#9348,#9349,
#9350));
#2248=EDGE_LOOP('',(#9351,#9352,#9353,#9354));
#2249=EDGE_LOOP('',(#9355,#9356,#9357,#9358,#9359,#9360));
#2250=EDGE_LOOP('',(#9361));
#2251=EDGE_LOOP('',(#9362,#9363,#9364,#9365));
#2252=EDGE_LOOP('',(#9366,#9367,#9368,#9369));
#2253=EDGE_LOOP('',(#9370));
#2254=EDGE_LOOP('',(#9371,#9372,#9373,#9374));
#2255=EDGE_LOOP('',(#9375,#9376,#9377,#9378));
#2256=EDGE_LOOP('',(#9379,#9380,#9381,#9382));
#2257=EDGE_LOOP('',(#9383,#9384,#9385,#9386));
#2258=EDGE_LOOP('',(#9387,#9388,#9389,#9390));
#2259=EDGE_LOOP('',(#9391,#9392,#9393,#9394));
#2260=EDGE_LOOP('',(#9395,#9396,#9397,#9398,#9399,#9400));
#2261=EDGE_LOOP('',(#9401));
#2262=EDGE_LOOP('',(#9402,#9403,#9404,#9405,#9406,#9407));
#2263=EDGE_LOOP('',(#9408,#9409,#9410,#9411));
#2264=EDGE_LOOP('',(#9412,#9413,#9414,#9415));
#2265=EDGE_LOOP('',(#9416,#9417,#9418,#9419));
#2266=EDGE_LOOP('',(#9420,#9421,#9422,#9423));
#2267=EDGE_LOOP('',(#9424,#9425,#9426,#9427,#9428));
#2268=EDGE_LOOP('',(#9429,#9430,#9431,#9432));
#2269=EDGE_LOOP('',(#9433,#9434,#9435,#9436));
#2270=EDGE_LOOP('',(#9437,#9438,#9439,#9440));
#2271=EDGE_LOOP('',(#9441,#9442,#9443,#9444));
#2272=EDGE_LOOP('',(#9445,#9446,#9447,#9448));
#2273=EDGE_LOOP('',(#9449,#9450,#9451,#9452,#9453));
#2274=EDGE_LOOP('',(#9454,#9455,#9456,#9457,#9458,#9459,#9460,#9461,#9462,
#9463,#9464,#9465,#9466,#9467,#9468,#9469,#9470,#9471));
#2275=EDGE_LOOP('',(#9472,#9473,#9474,#9475));
#2276=EDGE_LOOP('',(#9476,#9477,#9478,#9479));
#2277=EDGE_LOOP('',(#9480,#9481,#9482,#9483));
#2278=EDGE_LOOP('',(#9484,#9485,#9486,#9487,#9488,#9489,#9490,#9491,#9492,
#9493,#9494,#9495,#9496,#9497,#9498,#9499,#9500,#9501));
#2279=EDGE_LOOP('',(#9502,#9503,#9504,#9505,#9506,#9507));
#2280=EDGE_LOOP('',(#9508,#9509,#9510,#9511));
#2281=EDGE_LOOP('',(#9512,#9513,#9514,#9515,#9516,#9517));
#2282=EDGE_LOOP('',(#9518,#9519,#9520));
#2283=EDGE_LOOP('',(#9521,#9522,#9523,#9524,#9525));
#2284=EDGE_LOOP('',(#9526,#9527,#9528,#9529));
#2285=EDGE_LOOP('',(#9530,#9531,#9532,#9533));
#2286=EDGE_LOOP('',(#9534,#9535,#9536,#9537));
#2287=EDGE_LOOP('',(#9538,#9539,#9540,#9541,#9542));
#2288=EDGE_LOOP('',(#9543,#9544,#9545,#9546));
#2289=EDGE_LOOP('',(#9547,#9548,#9549,#9550));
#2290=EDGE_LOOP('',(#9551,#9552,#9553,#9554,#9555));
#2291=EDGE_LOOP('',(#9556,#9557,#9558,#9559,#9560,#9561));
#2292=EDGE_LOOP('',(#9562,#9563,#9564,#9565));
#2293=EDGE_LOOP('',(#9566));
#2294=EDGE_LOOP('',(#9567,#9568,#9569,#9570,#9571,#9572));
#2295=EDGE_LOOP('',(#9573,#9574,#9575,#9576));
#2296=EDGE_LOOP('',(#9577,#9578,#9579,#9580));
#2297=EDGE_LOOP('',(#9581,#9582,#9583,#9584));
#2298=EDGE_LOOP('',(#9585,#9586,#9587,#9588));
#2299=EDGE_LOOP('',(#9589,#9590,#9591,#9592));
#2300=EDGE_LOOP('',(#9593,#9594,#9595,#9596));
#2301=EDGE_LOOP('',(#9597,#9598,#9599,#9600));
#2302=EDGE_LOOP('',(#9601,#9602,#9603,#9604));
#2303=EDGE_LOOP('',(#9605));
#2304=EDGE_LOOP('',(#9606,#9607,#9608,#9609,#9610,#9611));
#2305=EDGE_LOOP('',(#9612));
#2306=EDGE_LOOP('',(#9613,#9614,#9615,#9616));
#2307=EDGE_LOOP('',(#9617,#9618,#9619,#9620));
#2308=EDGE_LOOP('',(#9621,#9622,#9623,#9624));
#2309=EDGE_LOOP('',(#9625,#9626,#9627,#9628));
#2310=EDGE_LOOP('',(#9629,#9630,#9631,#9632));
#2311=EDGE_LOOP('',(#9633,#9634,#9635,#9636));
#2312=EDGE_LOOP('',(#9637,#9638,#9639,#9640,#9641,#9642));
#2313=EDGE_LOOP('',(#9643));
#2314=EDGE_LOOP('',(#9644,#9645,#9646,#9647));
#2315=EDGE_LOOP('',(#9648,#9649,#9650,#9651,#9652,#9653));
#2316=EDGE_LOOP('',(#9654,#9655,#9656,#9657,#9658,#9659));
#2317=EDGE_LOOP('',(#9660,#9661,#9662,#9663,#9664,#9665));
#2318=EDGE_LOOP('',(#9666,#9667,#9668,#9669));
#2319=EDGE_LOOP('',(#9670,#9671,#9672,#9673,#9674,#9675));
#2320=EDGE_LOOP('',(#9676,#9677,#9678,#9679));
#2321=EDGE_LOOP('',(#9680,#9681,#9682,#9683));
#2322=EDGE_LOOP('',(#9684,#9685,#9686,#9687,#9688,#9689));
#2323=EDGE_LOOP('',(#9690,#9691,#9692,#9693));
#2324=EDGE_LOOP('',(#9694,#9695,#9696,#9697));
#2325=EDGE_LOOP('',(#9698,#9699,#9700,#9701,#9702,#9703));
#2326=EDGE_LOOP('',(#9704,#9705,#9706,#9707,#9708,#9709));
#2327=EDGE_LOOP('',(#9710,#9711,#9712,#9713,#9714,#9715));
#2328=EDGE_LOOP('',(#9716,#9717,#9718,#9719,#9720,#9721));
#2329=EDGE_LOOP('',(#9722,#9723,#9724,#9725));
#2330=EDGE_LOOP('',(#9726,#9727,#9728,#9729));
#2331=EDGE_LOOP('',(#9730,#9731,#9732,#9733,#9734,#9735));
#2332=EDGE_LOOP('',(#9736,#9737,#9738,#9739,#9740,#9741));
#2333=EDGE_LOOP('',(#9742,#9743,#9744,#9745,#9746,#9747));
#2334=EDGE_LOOP('',(#9748,#9749,#9750,#9751,#9752,#9753));
#2335=EDGE_LOOP('',(#9754,#9755,#9756,#9757));
#2336=EDGE_LOOP('',(#9758,#9759,#9760,#9761));
#2337=EDGE_LOOP('',(#9762,#9763,#9764,#9765,#9766,#9767));
#2338=EDGE_LOOP('',(#9768,#9769,#9770,#9771));
#2339=EDGE_LOOP('',(#9772));
#2340=EDGE_LOOP('',(#9773,#9774,#9775,#9776,#9777,#9778));
#2341=EDGE_LOOP('',(#9779,#9780,#9781,#9782,#9783,#9784));
#2342=EDGE_LOOP('',(#9785,#9786,#9787,#9788,#9789,#9790));
#2343=EDGE_LOOP('',(#9791,#9792,#9793,#9794));
#2344=EDGE_LOOP('',(#9795,#9796,#9797,#9798));
#2345=EDGE_LOOP('',(#9799,#9800,#9801,#9802));
#2346=EDGE_LOOP('',(#9803,#9804,#9805,#9806));
#2347=EDGE_LOOP('',(#9807,#9808,#9809,#9810));
#2348=EDGE_LOOP('',(#9811,#9812,#9813,#9814));
#2349=EDGE_LOOP('',(#9815,#9816,#9817,#9818));
#2350=EDGE_LOOP('',(#9819,#9820,#9821,#9822));
#2351=EDGE_LOOP('',(#9823));
#2352=EDGE_LOOP('',(#9824,#9825,#9826,#9827));
#2353=EDGE_LOOP('',(#9828,#9829,#9830,#9831,#9832,#9833));
#2354=EDGE_LOOP('',(#9834));
#2355=EDGE_LOOP('',(#9835,#9836,#9837,#9838));
#2356=EDGE_LOOP('',(#9839,#9840,#9841,#9842));
#2357=EDGE_LOOP('',(#9843,#9844,#9845,#9846));
#2358=EDGE_LOOP('',(#9847,#9848,#9849,#9850));
#2359=EDGE_LOOP('',(#9851,#9852,#9853,#9854));
#2360=EDGE_LOOP('',(#9855,#9856,#9857,#9858));
#2361=EDGE_LOOP('',(#9859,#9860,#9861,#9862));
#2362=EDGE_LOOP('',(#9863,#9864,#9865,#9866));
#2363=EDGE_LOOP('',(#9867,#9868,#9869,#9870));
#2364=EDGE_LOOP('',(#9871,#9872,#9873,#9874));
#2365=EDGE_LOOP('',(#9875,#9876,#9877,#9878,#9879,#9880));
#2366=EDGE_LOOP('',(#9881,#9882,#9883,#9884));
#2367=EDGE_LOOP('',(#9885,#9886,#9887,#9888));
#2368=EDGE_LOOP('',(#9889,#9890,#9891,#9892));
#2369=EDGE_LOOP('',(#9893,#9894,#9895,#9896));
#2370=EDGE_LOOP('',(#9897,#9898,#9899,#9900));
#2371=EDGE_LOOP('',(#9901,#9902,#9903,#9904));
#2372=EDGE_LOOP('',(#9905,#9906,#9907));
#2373=EDGE_LOOP('',(#9908,#9909,#9910,#9911));
#2374=EDGE_LOOP('',(#9912,#9913,#9914,#9915,#9916));
#2375=EDGE_LOOP('',(#9917,#9918,#9919,#9920,#9921));
#2376=EDGE_LOOP('',(#9922,#9923,#9924,#9925));
#2377=EDGE_LOOP('',(#9926,#9927,#9928,#9929));
#2378=EDGE_LOOP('',(#9930,#9931,#9932,#9933,#9934));
#2379=EDGE_LOOP('',(#9935,#9936,#9937,#9938));
#2380=EDGE_LOOP('',(#9939,#9940,#9941,#9942));
#2381=EDGE_LOOP('',(#9943,#9944,#9945,#9946));
#2382=EDGE_LOOP('',(#9947));
#2383=EDGE_LOOP('',(#9948,#9949,#9950,#9951));
#2384=EDGE_LOOP('',(#9952,#9953,#9954,#9955));
#2385=EDGE_LOOP('',(#9956,#9957,#9958,#9959));
#2386=EDGE_LOOP('',(#9960));
#2387=EDGE_LOOP('',(#9961,#9962,#9963,#9964));
#2388=EDGE_LOOP('',(#9965,#9966,#9967,#9968,#9969,#9970));
#2389=EDGE_LOOP('',(#9971));
#2390=EDGE_LOOP('',(#9972,#9973,#9974,#9975));
#2391=EDGE_LOOP('',(#9976,#9977,#9978,#9979));
#2392=EDGE_LOOP('',(#9980,#9981,#9982,#9983));
#2393=EDGE_LOOP('',(#9984,#9985,#9986,#9987));
#2394=EDGE_LOOP('',(#9988,#9989,#9990,#9991));
#2395=EDGE_LOOP('',(#9992,#9993,#9994,#9995));
#2396=EDGE_LOOP('',(#9996,#9997,#9998,#9999));
#2397=EDGE_LOOP('',(#10000,#10001,#10002,#10003));
#2398=EDGE_LOOP('',(#10004,#10005,#10006,#10007));
#2399=EDGE_LOOP('',(#10008,#10009,#10010,#10011));
#2400=EDGE_LOOP('',(#10012,#10013,#10014,#10015,#10016,#10017));
#2401=EDGE_LOOP('',(#10018));
#2402=EDGE_LOOP('',(#10019,#10020,#10021,#10022));
#2403=EDGE_LOOP('',(#10023,#10024,#10025,#10026));
#2404=EDGE_LOOP('',(#10027,#10028,#10029,#10030));
#2405=EDGE_LOOP('',(#10031,#10032,#10033,#10034));
#2406=EDGE_LOOP('',(#10035,#10036,#10037,#10038));
#2407=EDGE_LOOP('',(#10039,#10040,#10041,#10042));
#2408=EDGE_LOOP('',(#10043,#10044,#10045,#10046));
#2409=EDGE_LOOP('',(#10047,#10048,#10049,#10050));
#2410=EDGE_LOOP('',(#10051,#10052,#10053,#10054));
#2411=EDGE_LOOP('',(#10055,#10056,#10057,#10058));
#2412=EDGE_LOOP('',(#10059,#10060,#10061,#10062));
#2413=EDGE_LOOP('',(#10063,#10064,#10065,#10066));
#2414=EDGE_LOOP('',(#10067,#10068,#10069,#10070));
#2415=EDGE_LOOP('',(#10071,#10072,#10073,#10074,#10075,#10076));
#2416=EDGE_LOOP('',(#10077,#10078,#10079));
#2417=EDGE_LOOP('',(#10080,#10081,#10082,#10083));
#2418=EDGE_LOOP('',(#10084,#10085,#10086));
#2419=EDGE_LOOP('',(#10087,#10088,#10089,#10090));
#2420=EDGE_LOOP('',(#10091,#10092,#10093,#10094,#10095));
#2421=EDGE_LOOP('',(#10096,#10097,#10098,#10099));
#2422=EDGE_LOOP('',(#10100,#10101,#10102,#10103,#10104));
#2423=EDGE_LOOP('',(#10105,#10106,#10107,#10108));
#2424=EDGE_LOOP('',(#10109,#10110,#10111,#10112));
#2425=EDGE_LOOP('',(#10113,#10114,#10115,#10116,#10117));
#2426=EDGE_LOOP('',(#10118,#10119,#10120));
#2427=EDGE_LOOP('',(#10121,#10122,#10123,#10124));
#2428=EDGE_LOOP('',(#10125,#10126,#10127));
#2429=EDGE_LOOP('',(#10128,#10129,#10130,#10131));
#2430=EDGE_LOOP('',(#10132,#10133,#10134,#10135,#10136));
#2431=EDGE_LOOP('',(#10137,#10138,#10139,#10140));
#2432=EDGE_LOOP('',(#10141,#10142,#10143,#10144,#10145));
#2433=EDGE_LOOP('',(#10146,#10147,#10148,#10149));
#2434=EDGE_LOOP('',(#10150,#10151,#10152,#10153));
#2435=EDGE_LOOP('',(#10154,#10155,#10156,#10157,#10158));
#2436=EDGE_LOOP('',(#10159,#10160,#10161,#10162,#10163,#10164));
#2437=EDGE_LOOP('',(#10165,#10166,#10167,#10168));
#2438=EDGE_LOOP('',(#10169,#10170,#10171,#10172,#10173));
#2439=EDGE_LOOP('',(#10174,#10175,#10176,#10177));
#2440=EDGE_LOOP('',(#10178,#10179,#10180,#10181));
#2441=EDGE_LOOP('',(#10182,#10183,#10184,#10185));
#2442=EDGE_LOOP('',(#10186,#10187,#10188,#10189));
#2443=EDGE_LOOP('',(#10190,#10191,#10192,#10193));
#2444=EDGE_LOOP('',(#10194,#10195,#10196,#10197));
#2445=EDGE_LOOP('',(#10198,#10199,#10200,#10201,#10202,#10203,#10204,#10205,
#10206,#10207,#10208,#10209,#10210,#10211,#10212,#10213,#10214,#10215,#10216,
#10217));
#2446=EDGE_LOOP('',(#10218,#10219,#10220,#10221));
#2447=EDGE_LOOP('',(#10222,#10223,#10224,#10225));
#2448=EDGE_LOOP('',(#10226,#10227,#10228,#10229));
#2449=EDGE_LOOP('',(#10230,#10231,#10232,#10233));
#2450=EDGE_LOOP('',(#10234,#10235,#10236,#10237));
#2451=EDGE_LOOP('',(#10238,#10239,#10240,#10241));
#2452=EDGE_LOOP('',(#10242,#10243,#10244,#10245));
#2453=EDGE_LOOP('',(#10246,#10247,#10248,#10249));
#2454=EDGE_LOOP('',(#10250,#10251,#10252,#10253));
#2455=EDGE_LOOP('',(#10254,#10255,#10256,#10257));
#2456=EDGE_LOOP('',(#10258,#10259,#10260,#10261));
#2457=EDGE_LOOP('',(#10262));
#2458=EDGE_LOOP('',(#10263,#10264,#10265,#10266,#10267,#10268,#10269,#10270));
#2459=EDGE_LOOP('',(#10271,#10272,#10273,#10274,#10275,#10276,#10277,#10278));
#2460=EDGE_LOOP('',(#10279,#10280,#10281,#10282));
#2461=EDGE_LOOP('',(#10283,#10284,#10285,#10286));
#2462=EDGE_LOOP('',(#10287,#10288,#10289,#10290,#10291));
#2463=EDGE_LOOP('',(#10292,#10293,#10294,#10295));
#2464=EDGE_LOOP('',(#10296,#10297,#10298,#10299));
#2465=EDGE_LOOP('',(#10300,#10301,#10302,#10303));
#2466=EDGE_LOOP('',(#10304,#10305,#10306,#10307));
#2467=EDGE_LOOP('',(#10308,#10309,#10310,#10311));
#2468=EDGE_LOOP('',(#10312,#10313,#10314,#10315));
#2469=EDGE_LOOP('',(#10316,#10317,#10318,#10319));
#2470=EDGE_LOOP('',(#10320,#10321,#10322,#10323));
#2471=EDGE_LOOP('',(#10324,#10325,#10326,#10327));
#2472=EDGE_LOOP('',(#10328,#10329,#10330,#10331,#10332));
#2473=EDGE_LOOP('',(#10333,#10334,#10335,#10336,#10337,#10338));
#2474=EDGE_LOOP('',(#10339,#10340,#10341,#10342,#10343,#10344));
#2475=EDGE_LOOP('',(#10345,#10346,#10347,#10348,#10349));
#2476=EDGE_LOOP('',(#10350,#10351,#10352,#10353,#10354,#10355));
#2477=EDGE_LOOP('',(#10356,#10357,#10358,#10359));
#2478=EDGE_LOOP('',(#10360,#10361,#10362,#10363));
#2479=EDGE_LOOP('',(#10364,#10365,#10366,#10367));
#2480=EDGE_LOOP('',(#10368,#10369,#10370,#10371,#10372,#10373,#10374,#10375));
#2481=EDGE_LOOP('',(#10376,#10377,#10378,#10379));
#2482=EDGE_LOOP('',(#10380,#10381,#10382,#10383));
#2483=EDGE_LOOP('',(#10384,#10385,#10386,#10387,#10388,#10389,#10390,#10391,
#10392,#10393,#10394,#10395,#10396,#10397,#10398,#10399,#10400,#10401,#10402,
#10403,#10404,#10405,#10406,#10407,#10408,#10409));
#2484=EDGE_LOOP('',(#10410,#10411,#10412,#10413,#10414,#10415,#10416,#10417));
#2485=EDGE_LOOP('',(#10418,#10419,#10420,#10421,#10422,#10423,#10424,#10425));
#2486=EDGE_LOOP('',(#10426,#10427,#10428,#10429));
#2487=EDGE_LOOP('',(#10430,#10431,#10432,#10433));
#2488=EDGE_LOOP('',(#10434,#10435,#10436,#10437));
#2489=EDGE_LOOP('',(#10438,#10439,#10440,#10441,#10442));
#2490=EDGE_LOOP('',(#10443,#10444,#10445,#10446));
#2491=EDGE_LOOP('',(#10447,#10448,#10449,#10450));
#2492=EDGE_LOOP('',(#10451,#10452,#10453,#10454,#10455,#10456,#10457,#10458));
#2493=EDGE_LOOP('',(#10459,#10460,#10461,#10462,#10463));
#2494=EDGE_LOOP('',(#10464,#10465,#10466,#10467));
#2495=EDGE_LOOP('',(#10468,#10469,#10470,#10471));
#2496=EDGE_LOOP('',(#10472,#10473,#10474,#10475));
#2497=EDGE_LOOP('',(#10476,#10477,#10478,#10479,#10480,#10481,#10482,#10483));
#2498=EDGE_LOOP('',(#10484,#10485,#10486,#10487));
#2499=EDGE_LOOP('',(#10488,#10489,#10490,#10491));
#2500=EDGE_LOOP('',(#10492,#10493,#10494,#10495));
#2501=EDGE_LOOP('',(#10496,#10497,#10498,#10499));
#2502=EDGE_LOOP('',(#10500));
#2503=EDGE_LOOP('',(#10501));
#2504=EDGE_LOOP('',(#10502));
#2505=EDGE_LOOP('',(#10503,#10504,#10505,#10506));
#2506=EDGE_LOOP('',(#10507,#10508,#10509,#10510));
#2507=EDGE_LOOP('',(#10511,#10512,#10513,#10514));
#2508=EDGE_LOOP('',(#10515,#10516,#10517,#10518));
#2509=EDGE_LOOP('',(#10519,#10520,#10521,#10522));
#2510=EDGE_LOOP('',(#10523,#10524,#10525,#10526));
#2511=EDGE_LOOP('',(#10527,#10528,#10529,#10530));
#2512=EDGE_LOOP('',(#10531,#10532,#10533,#10534));
#2513=EDGE_LOOP('',(#10535,#10536,#10537,#10538));
#2514=EDGE_LOOP('',(#10539,#10540,#10541,#10542));
#2515=EDGE_LOOP('',(#10543,#10544,#10545,#10546));
#2516=EDGE_LOOP('',(#10547,#10548,#10549,#10550,#10551,#10552,#10553,#10554));
#2517=EDGE_LOOP('',(#10555));
#2518=EDGE_LOOP('',(#10556));
#2519=EDGE_LOOP('',(#10557));
#2520=EDGE_LOOP('',(#10558,#10559,#10560,#10561));
#2521=EDGE_LOOP('',(#10562,#10563,#10564,#10565,#10566,#10567,#10568,#10569));
#2522=EDGE_LOOP('',(#10570));
#2523=EDGE_LOOP('',(#10571));
#2524=EDGE_LOOP('',(#10572));
#2525=EDGE_LOOP('',(#10573,#10574,#10575,#10576));
#2526=EDGE_LOOP('',(#10577,#10578,#10579,#10580));
#2527=EDGE_LOOP('',(#10581,#10582,#10583,#10584));
#2528=EDGE_LOOP('',(#10585,#10586,#10587,#10588));
#2529=EDGE_LOOP('',(#10589,#10590,#10591,#10592));
#2530=EDGE_LOOP('',(#10593,#10594,#10595,#10596));
#2531=EDGE_LOOP('',(#10597,#10598,#10599,#10600));
#2532=EDGE_LOOP('',(#10601,#10602,#10603,#10604));
#2533=EDGE_LOOP('',(#10605,#10606,#10607,#10608));
#2534=EDGE_LOOP('',(#10609,#10610,#10611,#10612));
#2535=EDGE_LOOP('',(#10613,#10614,#10615,#10616));
#2536=EDGE_LOOP('',(#10617,#10618,#10619,#10620));
#2537=EDGE_LOOP('',(#10621,#10622,#10623,#10624));
#2538=EDGE_LOOP('',(#10625,#10626,#10627,#10628));
#2539=EDGE_LOOP('',(#10629,#10630,#10631,#10632));
#2540=EDGE_LOOP('',(#10633,#10634,#10635,#10636));
#2541=EDGE_LOOP('',(#10637,#10638,#10639,#10640));
#2542=EDGE_LOOP('',(#10641,#10642,#10643,#10644));
#2543=EDGE_LOOP('',(#10645,#10646,#10647,#10648));
#2544=EDGE_LOOP('',(#10649,#10650,#10651,#10652));
#2545=EDGE_LOOP('',(#10653,#10654,#10655,#10656));
#2546=EDGE_LOOP('',(#10657,#10658,#10659,#10660));
#2547=EDGE_LOOP('',(#10661,#10662,#10663,#10664));
#2548=EDGE_LOOP('',(#10665,#10666,#10667,#10668));
#2549=EDGE_LOOP('',(#10669,#10670,#10671,#10672));
#2550=EDGE_LOOP('',(#10673,#10674,#10675,#10676));
#2551=EDGE_LOOP('',(#10677,#10678,#10679,#10680));
#2552=EDGE_LOOP('',(#10681,#10682,#10683,#10684));
#2553=EDGE_LOOP('',(#10685,#10686,#10687,#10688));
#2554=EDGE_LOOP('',(#10689,#10690,#10691,#10692));
#2555=EDGE_LOOP('',(#10693,#10694,#10695,#10696));
#2556=EDGE_LOOP('',(#10697,#10698,#10699,#10700));
#2557=EDGE_LOOP('',(#10701,#10702,#10703,#10704));
#2558=EDGE_LOOP('',(#10705,#10706,#10707,#10708));
#2559=EDGE_LOOP('',(#10709,#10710,#10711,#10712));
#2560=EDGE_LOOP('',(#10713,#10714,#10715,#10716));
#2561=EDGE_LOOP('',(#10717,#10718,#10719,#10720));
#2562=EDGE_LOOP('',(#10721,#10722,#10723,#10724));
#2563=EDGE_LOOP('',(#10725,#10726,#10727,#10728));
#2564=EDGE_LOOP('',(#10729,#10730,#10731,#10732));
#2565=EDGE_LOOP('',(#10733,#10734,#10735,#10736));
#2566=EDGE_LOOP('',(#10737,#10738,#10739,#10740));
#2567=EDGE_LOOP('',(#10741,#10742,#10743,#10744));
#2568=EDGE_LOOP('',(#10745,#10746,#10747,#10748));
#2569=EDGE_LOOP('',(#10749,#10750,#10751,#10752));
#2570=EDGE_LOOP('',(#10753,#10754,#10755,#10756));
#2571=EDGE_LOOP('',(#10757,#10758,#10759,#10760));
#2572=EDGE_LOOP('',(#10761,#10762,#10763,#10764));
#2573=EDGE_LOOP('',(#10765,#10766,#10767,#10768));
#2574=EDGE_LOOP('',(#10769,#10770,#10771,#10772));
#2575=EDGE_LOOP('',(#10773,#10774,#10775,#10776));
#2576=EDGE_LOOP('',(#10777,#10778,#10779,#10780));
#2577=EDGE_LOOP('',(#10781,#10782,#10783,#10784));
#2578=EDGE_LOOP('',(#10785,#10786,#10787,#10788));
#2579=EDGE_LOOP('',(#10789,#10790,#10791,#10792));
#2580=EDGE_LOOP('',(#10793,#10794,#10795,#10796));
#2581=EDGE_LOOP('',(#10797,#10798,#10799,#10800));
#2582=EDGE_LOOP('',(#10801,#10802,#10803,#10804));
#2583=EDGE_LOOP('',(#10805,#10806,#10807,#10808));
#2584=EDGE_LOOP('',(#10809,#10810,#10811,#10812));
#2585=EDGE_LOOP('',(#10813,#10814,#10815,#10816));
#2586=EDGE_LOOP('',(#10817,#10818,#10819,#10820));
#2587=EDGE_LOOP('',(#10821,#10822,#10823,#10824));
#2588=EDGE_LOOP('',(#10825,#10826,#10827,#10828));
#2589=EDGE_LOOP('',(#10829,#10830,#10831,#10832));
#2590=EDGE_LOOP('',(#10833,#10834,#10835,#10836));
#2591=EDGE_LOOP('',(#10837,#10838,#10839));
#2592=EDGE_LOOP('',(#10840,#10841,#10842));
#2593=EDGE_LOOP('',(#10843,#10844,#10845));
#2594=EDGE_LOOP('',(#10846,#10847,#10848));
#2595=EDGE_LOOP('',(#10849,#10850,#10851));
#2596=EDGE_LOOP('',(#10852,#10853,#10854));
#2597=EDGE_LOOP('',(#10855,#10856,#10857));
#2598=EDGE_LOOP('',(#10858,#10859,#10860,#10861));
#2599=EDGE_LOOP('',(#10862,#10863,#10864));
#2600=EDGE_LOOP('',(#10865,#10866,#10867,#10868));
#2601=EDGE_LOOP('',(#10869,#10870,#10871,#10872));
#2602=EDGE_LOOP('',(#10873,#10874,#10875,#10876));
#2603=EDGE_LOOP('',(#10877,#10878,#10879,#10880));
#2604=EDGE_LOOP('',(#10881,#10882,#10883,#10884));
#2605=EDGE_LOOP('',(#10885,#10886,#10887,#10888));
#2606=EDGE_LOOP('',(#10889,#10890,#10891,#10892));
#2607=EDGE_LOOP('',(#10893,#10894,#10895,#10896));
#2608=EDGE_LOOP('',(#10897,#10898,#10899,#10900));
#2609=EDGE_LOOP('',(#10901,#10902,#10903,#10904));
#2610=EDGE_LOOP('',(#10905,#10906,#10907,#10908));
#2611=EDGE_LOOP('',(#10909,#10910,#10911,#10912));
#2612=EDGE_LOOP('',(#10913,#10914,#10915,#10916));
#2613=EDGE_LOOP('',(#10917,#10918,#10919,#10920));
#2614=EDGE_LOOP('',(#10921));
#2615=EDGE_LOOP('',(#10922,#10923,#10924,#10925));
#2616=EDGE_LOOP('',(#10926,#10927,#10928,#10929));
#2617=EDGE_LOOP('',(#10930));
#2618=EDGE_LOOP('',(#10931,#10932,#10933,#10934));
#2619=EDGE_LOOP('',(#10935,#10936,#10937,#10938));
#2620=EDGE_LOOP('',(#10939,#10940,#10941,#10942));
#2621=EDGE_LOOP('',(#10943,#10944,#10945,#10946));
#2622=EDGE_LOOP('',(#10947,#10948,#10949,#10950));
#2623=EDGE_LOOP('',(#10951,#10952,#10953,#10954));
#2624=EDGE_LOOP('',(#10955,#10956,#10957,#10958));
#2625=EDGE_LOOP('',(#10959,#10960,#10961,#10962));
#2626=EDGE_LOOP('',(#10963,#10964,#10965,#10966));
#2627=EDGE_LOOP('',(#10967,#10968,#10969,#10970));
#2628=EDGE_LOOP('',(#10971,#10972,#10973,#10974));
#2629=EDGE_LOOP('',(#10975,#10976,#10977,#10978));
#2630=EDGE_LOOP('',(#10979,#10980,#10981,#10982));
#2631=EDGE_LOOP('',(#10983,#10984,#10985,#10986));
#2632=EDGE_LOOP('',(#10987,#10988,#10989,#10990));
#2633=EDGE_LOOP('',(#10991,#10992,#10993,#10994));
#2634=EDGE_LOOP('',(#10995,#10996,#10997,#10998));
#2635=EDGE_LOOP('',(#10999,#11000,#11001,#11002));
#2636=EDGE_LOOP('',(#11003,#11004,#11005,#11006));
#2637=EDGE_LOOP('',(#11007,#11008,#11009,#11010));
#2638=EDGE_LOOP('',(#11011,#11012,#11013,#11014));
#2639=EDGE_LOOP('',(#11015,#11016,#11017,#11018));
#2640=EDGE_LOOP('',(#11019,#11020,#11021,#11022));
#2641=EDGE_LOOP('',(#11023,#11024,#11025,#11026));
#2642=EDGE_LOOP('',(#11027,#11028,#11029,#11030));
#2643=EDGE_LOOP('',(#11031,#11032,#11033,#11034));
#2644=EDGE_LOOP('',(#11035,#11036,#11037,#11038));
#2645=EDGE_LOOP('',(#11039,#11040,#11041,#11042));
#2646=EDGE_LOOP('',(#11043,#11044,#11045,#11046));
#2647=EDGE_LOOP('',(#11047,#11048,#11049,#11050));
#2648=EDGE_LOOP('',(#11051,#11052,#11053,#11054));
#2649=EDGE_LOOP('',(#11055,#11056,#11057,#11058));
#2650=EDGE_LOOP('',(#11059,#11060,#11061,#11062));
#2651=EDGE_LOOP('',(#11063,#11064,#11065,#11066));
#2652=EDGE_LOOP('',(#11067,#11068,#11069,#11070));
#2653=EDGE_LOOP('',(#11071,#11072,#11073,#11074));
#2654=EDGE_LOOP('',(#11075,#11076,#11077,#11078));
#2655=EDGE_LOOP('',(#11079,#11080,#11081,#11082));
#2656=EDGE_LOOP('',(#11083,#11084,#11085,#11086));
#2657=EDGE_LOOP('',(#11087,#11088,#11089,#11090));
#2658=EDGE_LOOP('',(#11091,#11092,#11093,#11094));
#2659=EDGE_LOOP('',(#11095,#11096,#11097,#11098));
#2660=EDGE_LOOP('',(#11099,#11100,#11101,#11102));
#2661=EDGE_LOOP('',(#11103,#11104,#11105,#11106));
#2662=EDGE_LOOP('',(#11107,#11108,#11109,#11110));
#2663=EDGE_LOOP('',(#11111,#11112,#11113,#11114));
#2664=EDGE_LOOP('',(#11115,#11116,#11117,#11118));
#2665=EDGE_LOOP('',(#11119,#11120,#11121,#11122));
#2666=EDGE_LOOP('',(#11123,#11124,#11125,#11126));
#2667=EDGE_LOOP('',(#11127,#11128,#11129,#11130));
#2668=EDGE_LOOP('',(#11131,#11132,#11133,#11134));
#2669=EDGE_LOOP('',(#11135,#11136,#11137,#11138));
#2670=EDGE_LOOP('',(#11139,#11140,#11141,#11142));
#2671=EDGE_LOOP('',(#11143,#11144,#11145,#11146));
#2672=EDGE_LOOP('',(#11147,#11148,#11149,#11150));
#2673=EDGE_LOOP('',(#11151,#11152,#11153,#11154));
#2674=EDGE_LOOP('',(#11155,#11156,#11157,#11158));
#2675=EDGE_LOOP('',(#11159,#11160,#11161,#11162,#11163,#11164,#11165,#11166,
#11167,#11168,#11169,#11170,#11171,#11172,#11173,#11174,#11175,#11176,#11177,
#11178,#11179,#11180,#11181,#11182,#11183,#11184,#11185,#11186,#11187,#11188,
#11189,#11190,#11191,#11192,#11193,#11194,#11195,#11196,#11197,#11198,#11199,
#11200,#11201,#11202,#11203,#11204,#11205,#11206,#11207,#11208,#11209,#11210));
#2676=EDGE_LOOP('',(#11211,#11212,#11213,#11214,#11215,#11216,#11217,#11218,
#11219,#11220,#11221,#11222,#11223,#11224,#11225,#11226,#11227,#11228,#11229,
#11230,#11231,#11232,#11233,#11234,#11235,#11236,#11237,#11238,#11239,#11240,
#11241,#11242,#11243,#11244,#11245,#11246,#11247,#11248,#11249,#11250,#11251,
#11252,#11253,#11254,#11255,#11256,#11257,#11258,#11259,#11260,#11261,#11262,
#11263,#11264,#11265,#11266,#11267,#11268,#11269,#11270,#11271,#11272,#11273,
#11274,#11275,#11276,#11277,#11278,#11279,#11280,#11281,#11282,#11283,#11284,
#11285,#11286,#11287,#11288,#11289,#11290,#11291,#11292,#11293,#11294,#11295,
#11296,#11297,#11298,#11299,#11300,#11301,#11302,#11303,#11304,#11305,#11306,
#11307,#11308,#11309,#11310));
#2677=EDGE_LOOP('',(#11311));
#2678=EDGE_LOOP('',(#11312,#11313,#11314,#11315));
#2679=EDGE_LOOP('',(#11316,#11317,#11318,#11319,#11320,#11321,#11322,#11323,
#11324,#11325,#11326,#11327,#11328,#11329,#11330,#11331,#11332,#11333,#11334,
#11335,#11336,#11337,#11338,#11339,#11340,#11341,#11342,#11343,#11344,#11345,
#11346,#11347,#11348,#11349,#11350,#11351,#11352,#11353,#11354,#11355,#11356,
#11357,#11358,#11359,#11360,#11361,#11362,#11363,#11364,#11365,#11366,#11367,
#11368,#11369,#11370,#11371,#11372,#11373,#11374));
#2680=EDGE_LOOP('',(#11375,#11376,#11377,#11378,#11379));
#2681=EDGE_LOOP('',(#11380,#11381,#11382,#11383));
#2682=EDGE_LOOP('',(#11384,#11385,#11386,#11387,#11388,#11389,#11390,#11391,
#11392,#11393,#11394,#11395,#11396,#11397,#11398,#11399,#11400,#11401,#11402,
#11403,#11404,#11405,#11406,#11407,#11408,#11409,#11410,#11411,#11412,#11413,
#11414,#11415,#11416,#11417,#11418,#11419,#11420,#11421,#11422,#11423,#11424,
#11425,#11426,#11427,#11428,#11429,#11430,#11431,#11432,#11433,#11434,#11435,
#11436,#11437,#11438,#11439,#11440,#11441,#11442));
#2683=EDGE_LOOP('',(#11443,#11444,#11445,#11446));
#2684=EDGE_LOOP('',(#11447,#11448,#11449));
#2685=EDGE_LOOP('',(#11450,#11451,#11452,#11453));
#2686=EDGE_LOOP('',(#11454,#11455,#11456));
#2687=EDGE_LOOP('',(#11457,#11458,#11459,#11460));
#2688=EDGE_LOOP('',(#11461,#11462,#11463));
#2689=EDGE_LOOP('',(#11464,#11465,#11466,#11467));
#2690=EDGE_LOOP('',(#11468,#11469,#11470));
#2691=EDGE_LOOP('',(#11471,#11472,#11473,#11474));
#2692=EDGE_LOOP('',(#11475,#11476,#11477));
#2693=EDGE_LOOP('',(#11478,#11479,#11480,#11481));
#2694=EDGE_LOOP('',(#11482,#11483,#11484));
#2695=EDGE_LOOP('',(#11485,#11486,#11487,#11488));
#2696=EDGE_LOOP('',(#11489,#11490,#11491));
#2697=EDGE_LOOP('',(#11492,#11493,#11494,#11495));
#2698=EDGE_LOOP('',(#11496,#11497,#11498));
#2699=EDGE_LOOP('',(#11499,#11500,#11501,#11502));
#2700=EDGE_LOOP('',(#11503,#11504,#11505));
#2701=EDGE_LOOP('',(#11506,#11507,#11508,#11509));
#2702=EDGE_LOOP('',(#11510,#11511,#11512));
#2703=EDGE_LOOP('',(#11513,#11514,#11515,#11516));
#2704=EDGE_LOOP('',(#11517,#11518,#11519));
#2705=EDGE_LOOP('',(#11520,#11521,#11522,#11523));
#2706=EDGE_LOOP('',(#11524,#11525,#11526));
#2707=EDGE_LOOP('',(#11527,#11528,#11529,#11530));
#2708=EDGE_LOOP('',(#11531,#11532,#11533));
#2709=EDGE_LOOP('',(#11534,#11535,#11536,#11537));
#2710=EDGE_LOOP('',(#11538,#11539,#11540));
#2711=EDGE_LOOP('',(#11541,#11542,#11543,#11544));
#2712=EDGE_LOOP('',(#11545,#11546,#11547));
#2713=EDGE_LOOP('',(#11548,#11549,#11550,#11551));
#2714=EDGE_LOOP('',(#11552,#11553,#11554));
#2715=EDGE_LOOP('',(#11555,#11556,#11557,#11558));
#2716=EDGE_LOOP('',(#11559,#11560,#11561));
#2717=EDGE_LOOP('',(#11562,#11563,#11564,#11565));
#2718=EDGE_LOOP('',(#11566,#11567,#11568));
#2719=EDGE_LOOP('',(#11569,#11570,#11571,#11572));
#2720=EDGE_LOOP('',(#11573,#11574,#11575));
#2721=EDGE_LOOP('',(#11576,#11577,#11578,#11579));
#2722=EDGE_LOOP('',(#11580,#11581,#11582));
#2723=EDGE_LOOP('',(#11583,#11584,#11585,#11586));
#2724=EDGE_LOOP('',(#11587,#11588,#11589));
#2725=EDGE_LOOP('',(#11590,#11591,#11592,#11593));
#2726=EDGE_LOOP('',(#11594,#11595,#11596));
#2727=EDGE_LOOP('',(#11597,#11598,#11599,#11600));
#2728=EDGE_LOOP('',(#11601,#11602,#11603));
#2729=EDGE_LOOP('',(#11604,#11605,#11606,#11607));
#2730=EDGE_LOOP('',(#11608,#11609,#11610,#11611));
#2731=EDGE_LOOP('',(#11612,#11613,#11614,#11615));
#2732=EDGE_LOOP('',(#11616,#11617,#11618));
#2733=EDGE_LOOP('',(#11619,#11620,#11621,#11622));
#2734=EDGE_LOOP('',(#11623,#11624,#11625));
#2735=EDGE_LOOP('',(#11626,#11627,#11628,#11629));
#2736=EDGE_LOOP('',(#11630,#11631,#11632));
#2737=EDGE_LOOP('',(#11633,#11634,#11635,#11636));
#2738=EDGE_LOOP('',(#11637,#11638,#11639));
#2739=EDGE_LOOP('',(#11640,#11641,#11642,#11643));
#2740=EDGE_LOOP('',(#11644,#11645,#11646));
#2741=EDGE_LOOP('',(#11647,#11648,#11649,#11650));
#2742=EDGE_LOOP('',(#11651,#11652,#11653));
#2743=EDGE_LOOP('',(#11654,#11655,#11656,#11657));
#2744=EDGE_LOOP('',(#11658,#11659,#11660));
#2745=EDGE_LOOP('',(#11661,#11662,#11663,#11664));
#2746=EDGE_LOOP('',(#11665,#11666,#11667));
#2747=EDGE_LOOP('',(#11668,#11669,#11670,#11671));
#2748=EDGE_LOOP('',(#11672,#11673,#11674));
#2749=EDGE_LOOP('',(#11675,#11676,#11677,#11678));
#2750=EDGE_LOOP('',(#11679,#11680,#11681));
#2751=EDGE_LOOP('',(#11682,#11683,#11684,#11685));
#2752=EDGE_LOOP('',(#11686,#11687,#11688));
#2753=EDGE_LOOP('',(#11689,#11690,#11691,#11692));
#2754=EDGE_LOOP('',(#11693,#11694,#11695));
#2755=EDGE_LOOP('',(#11696,#11697,#11698,#11699));
#2756=EDGE_LOOP('',(#11700,#11701,#11702));
#2757=EDGE_LOOP('',(#11703,#11704,#11705,#11706));
#2758=EDGE_LOOP('',(#11707,#11708,#11709));
#2759=EDGE_LOOP('',(#11710,#11711,#11712,#11713));
#2760=EDGE_LOOP('',(#11714,#11715,#11716));
#2761=EDGE_LOOP('',(#11717,#11718,#11719,#11720));
#2762=EDGE_LOOP('',(#11721,#11722,#11723));
#2763=EDGE_LOOP('',(#11724,#11725,#11726,#11727));
#2764=EDGE_LOOP('',(#11728,#11729,#11730));
#2765=EDGE_LOOP('',(#11731,#11732,#11733,#11734));
#2766=EDGE_LOOP('',(#11735,#11736,#11737));
#2767=EDGE_LOOP('',(#11738,#11739,#11740,#11741));
#2768=EDGE_LOOP('',(#11742,#11743,#11744));
#2769=EDGE_LOOP('',(#11745,#11746,#11747,#11748));
#2770=EDGE_LOOP('',(#11749,#11750,#11751));
#2771=EDGE_LOOP('',(#11752,#11753,#11754,#11755));
#2772=EDGE_LOOP('',(#11756,#11757,#11758));
#2773=EDGE_LOOP('',(#11759,#11760,#11761,#11762));
#2774=EDGE_LOOP('',(#11763,#11764,#11765));
#2775=EDGE_LOOP('',(#11766,#11767,#11768,#11769));
#2776=EDGE_LOOP('',(#11770,#11771,#11772,#11773));
#2777=EDGE_LOOP('',(#11774,#11775,#11776,#11777));
#2778=EDGE_LOOP('',(#11778,#11779,#11780));
#2779=EDGE_LOOP('',(#11781));
#2780=EDGE_LOOP('',(#11782,#11783,#11784,#11785,#11786,#11787));
#2781=EDGE_LOOP('',(#11788,#11789,#11790,#11791));
#2782=EDGE_LOOP('',(#11792,#11793,#11794,#11795));
#2783=EDGE_LOOP('',(#11796));
#2784=EDGE_LOOP('',(#11797));
#2785=EDGE_LOOP('',(#11798,#11799,#11800,#11801));
#2786=EDGE_LOOP('',(#11802));
#2787=EDGE_LOOP('',(#11803,#11804,#11805,#11806,#11807));
#2788=EDGE_LOOP('',(#11808,#11809,#11810,#11811,#11812));
#2789=EDGE_LOOP('',(#11813));
#2790=EDGE_LOOP('',(#11814));
#2791=EDGE_LOOP('',(#11815,#11816,#11817,#11818));
#2792=EDGE_LOOP('',(#11819,#11820,#11821,#11822,#11823,#11824,#11825,#11826,
#11827,#11828,#11829,#11830,#11831,#11832,#11833,#11834,#11835,#11836,#11837,
#11838,#11839,#11840,#11841,#11842,#11843,#11844,#11845,#11846,#11847,#11848,
#11849,#11850,#11851,#11852,#11853,#11854,#11855,#11856,#11857,#11858,#11859,
#11860,#11861,#11862,#11863,#11864,#11865,#11866,#11867,#11868,#11869,#11870,
#11871,#11872,#11873,#11874,#11875,#11876,#11877,#11878,#11879,#11880,#11881,
#11882,#11883,#11884,#11885,#11886,#11887,#11888));
#2793=EDGE_LOOP('',(#11889,#11890,#11891,#11892,#11893,#11894,#11895,#11896,
#11897,#11898,#11899,#11900,#11901,#11902,#11903,#11904,#11905,#11906,#11907,
#11908,#11909,#11910,#11911,#11912,#11913,#11914,#11915,#11916,#11917,#11918,
#11919,#11920,#11921,#11922,#11923,#11924,#11925,#11926,#11927,#11928,#11929,
#11930,#11931,#11932,#11933,#11934,#11935,#11936,#11937,#11938,#11939,#11940,
#11941,#11942,#11943,#11944,#11945,#11946,#11947,#11948,#11949,#11950,#11951,
#11952,#11953,#11954));
#2794=EDGE_LOOP('',(#11955,#11956,#11957,#11958));
#2795=EDGE_LOOP('',(#11959,#11960,#11961,#11962));
#2796=EDGE_LOOP('',(#11963,#11964,#11965,#11966));
#2797=EDGE_LOOP('',(#11967,#11968,#11969,#11970));
#2798=EDGE_LOOP('',(#11971,#11972,#11973,#11974));
#2799=EDGE_LOOP('',(#11975,#11976,#11977,#11978));
#2800=EDGE_LOOP('',(#11979,#11980,#11981,#11982));
#2801=EDGE_LOOP('',(#11983,#11984,#11985,#11986));
#2802=EDGE_LOOP('',(#11987,#11988,#11989,#11990));
#2803=EDGE_LOOP('',(#11991,#11992,#11993,#11994));
#2804=EDGE_LOOP('',(#11995,#11996,#11997,#11998));
#2805=EDGE_LOOP('',(#11999,#12000,#12001,#12002));
#2806=EDGE_LOOP('',(#12003,#12004,#12005,#12006));
#2807=EDGE_LOOP('',(#12007,#12008,#12009,#12010));
#2808=EDGE_LOOP('',(#12011,#12012,#12013,#12014));
#2809=EDGE_LOOP('',(#12015,#12016,#12017,#12018));
#2810=EDGE_LOOP('',(#12019,#12020,#12021,#12022));
#2811=EDGE_LOOP('',(#12023,#12024,#12025,#12026));
#2812=EDGE_LOOP('',(#12027,#12028,#12029,#12030));
#2813=EDGE_LOOP('',(#12031,#12032,#12033,#12034));
#2814=EDGE_LOOP('',(#12035,#12036,#12037,#12038));
#2815=EDGE_LOOP('',(#12039,#12040,#12041,#12042));
#2816=EDGE_LOOP('',(#12043,#12044,#12045,#12046));
#2817=EDGE_LOOP('',(#12047,#12048,#12049,#12050));
#2818=EDGE_LOOP('',(#12051,#12052,#12053,#12054));
#2819=EDGE_LOOP('',(#12055,#12056,#12057,#12058));
#2820=EDGE_LOOP('',(#12059,#12060,#12061,#12062));
#2821=EDGE_LOOP('',(#12063,#12064,#12065,#12066));
#2822=EDGE_LOOP('',(#12067,#12068,#12069,#12070));
#2823=EDGE_LOOP('',(#12071,#12072,#12073,#12074,#12075,#12076));
#2824=EDGE_LOOP('',(#12077,#12078,#12079,#12080));
#2825=EDGE_LOOP('',(#12081,#12082,#12083,#12084));
#2826=EDGE_LOOP('',(#12085,#12086,#12087,#12088));
#2827=EDGE_LOOP('',(#12089,#12090,#12091,#12092));
#2828=EDGE_LOOP('',(#12093,#12094,#12095,#12096,#12097,#12098));
#2829=EDGE_LOOP('',(#12099));
#2830=EDGE_LOOP('',(#12100,#12101,#12102,#12103));
#2831=EDGE_LOOP('',(#12104,#12105,#12106,#12107));
#2832=EDGE_LOOP('',(#12108,#12109,#12110,#12111));
#2833=EDGE_LOOP('',(#12112,#12113,#12114,#12115));
#2834=EDGE_LOOP('',(#12116,#12117,#12118,#12119));
#2835=EDGE_LOOP('',(#12120,#12121,#12122,#12123));
#2836=EDGE_LOOP('',(#12124,#12125,#12126,#12127));
#2837=EDGE_LOOP('',(#12128,#12129,#12130,#12131));
#2838=EDGE_LOOP('',(#12132,#12133,#12134,#12135));
#2839=EDGE_LOOP('',(#12136));
#2840=EDGE_LOOP('',(#12137,#12138,#12139,#12140,#12141,#12142));
#2841=EDGE_LOOP('',(#12143,#12144,#12145,#12146));
#2842=EDGE_LOOP('',(#12147,#12148,#12149,#12150));
#2843=EDGE_LOOP('',(#12151,#12152,#12153,#12154));
#2844=EDGE_LOOP('',(#12155,#12156,#12157,#12158));
#2845=EDGE_LOOP('',(#12159,#12160,#12161,#12162));
#2846=EDGE_LOOP('',(#12163,#12164,#12165,#12166));
#2847=EDGE_LOOP('',(#12167,#12168,#12169,#12170));
#2848=EDGE_LOOP('',(#12171,#12172,#12173,#12174));
#2849=EDGE_LOOP('',(#12175,#12176,#12177,#12178));
#2850=EDGE_LOOP('',(#12179,#12180,#12181,#12182));
#2851=EDGE_LOOP('',(#12183,#12184,#12185,#12186));
#2852=EDGE_LOOP('',(#12187,#12188,#12189,#12190));
#2853=EDGE_LOOP('',(#12191,#12192,#12193,#12194));
#2854=EDGE_LOOP('',(#12195,#12196,#12197,#12198));
#2855=EDGE_LOOP('',(#12199,#12200,#12201,#12202));
#2856=EDGE_LOOP('',(#12203,#12204,#12205,#12206));
#2857=EDGE_LOOP('',(#12207,#12208,#12209,#12210,#12211));
#2858=EDGE_LOOP('',(#12212,#12213,#12214,#12215,#12216));
#2859=EDGE_LOOP('',(#12217,#12218,#12219,#12220));
#2860=EDGE_LOOP('',(#12221,#12222,#12223,#12224));
#2861=EDGE_LOOP('',(#12225,#12226,#12227,#12228));
#2862=EDGE_LOOP('',(#12229,#12230,#12231,#12232));
#2863=EDGE_LOOP('',(#12233,#12234,#12235,#12236));
#2864=EDGE_LOOP('',(#12237,#12238,#12239,#12240));
#2865=EDGE_LOOP('',(#12241,#12242,#12243,#12244));
#2866=EDGE_LOOP('',(#12245,#12246,#12247,#12248));
#2867=EDGE_LOOP('',(#12249,#12250,#12251,#12252));
#2868=EDGE_LOOP('',(#12253,#12254,#12255,#12256));
#2869=EDGE_LOOP('',(#12257,#12258,#12259,#12260));
#2870=EDGE_LOOP('',(#12261,#12262,#12263,#12264));
#2871=EDGE_LOOP('',(#12265,#12266,#12267,#12268));
#2872=EDGE_LOOP('',(#12269,#12270,#12271,#12272));
#2873=EDGE_LOOP('',(#12273,#12274,#12275,#12276));
#2874=EDGE_LOOP('',(#12277,#12278,#12279,#12280));
#2875=EDGE_LOOP('',(#12281,#12282,#12283,#12284));
#2876=EDGE_LOOP('',(#12285,#12286,#12287,#12288));
#2877=EDGE_LOOP('',(#12289,#12290,#12291,#12292));
#2878=EDGE_LOOP('',(#12293,#12294,#12295,#12296));
#2879=EDGE_LOOP('',(#12297,#12298,#12299,#12300));
#2880=EDGE_LOOP('',(#12301,#12302,#12303,#12304));
#2881=EDGE_LOOP('',(#12305,#12306,#12307,#12308));
#2882=EDGE_LOOP('',(#12309,#12310,#12311,#12312));
#2883=EDGE_LOOP('',(#12313,#12314,#12315,#12316));
#2884=EDGE_LOOP('',(#12317,#12318,#12319,#12320));
#2885=EDGE_LOOP('',(#12321,#12322,#12323,#12324));
#2886=EDGE_LOOP('',(#12325,#12326,#12327,#12328));
#2887=EDGE_LOOP('',(#12329,#12330,#12331,#12332));
#2888=EDGE_LOOP('',(#12333,#12334,#12335,#12336));
#2889=EDGE_LOOP('',(#12337,#12338,#12339,#12340));
#2890=EDGE_LOOP('',(#12341,#12342,#12343,#12344));
#2891=EDGE_LOOP('',(#12345,#12346,#12347,#12348));
#2892=EDGE_LOOP('',(#12349,#12350,#12351,#12352));
#2893=EDGE_LOOP('',(#12353,#12354,#12355,#12356));
#2894=EDGE_LOOP('',(#12357,#12358,#12359,#12360));
#2895=EDGE_LOOP('',(#12361,#12362,#12363,#12364));
#2896=EDGE_LOOP('',(#12365,#12366,#12367,#12368));
#2897=EDGE_LOOP('',(#12369,#12370,#12371,#12372));
#2898=EDGE_LOOP('',(#12373,#12374,#12375,#12376));
#2899=EDGE_LOOP('',(#12377,#12378,#12379,#12380));
#2900=EDGE_LOOP('',(#12381,#12382,#12383,#12384));
#2901=EDGE_LOOP('',(#12385,#12386,#12387,#12388));
#2902=EDGE_LOOP('',(#12389,#12390,#12391,#12392));
#2903=EDGE_LOOP('',(#12393,#12394,#12395,#12396));
#2904=EDGE_LOOP('',(#12397,#12398,#12399,#12400));
#2905=EDGE_LOOP('',(#12401,#12402,#12403,#12404));
#2906=EDGE_LOOP('',(#12405,#12406,#12407,#12408));
#2907=EDGE_LOOP('',(#12409,#12410,#12411,#12412));
#2908=EDGE_LOOP('',(#12413,#12414,#12415,#12416));
#2909=EDGE_LOOP('',(#12417,#12418,#12419,#12420));
#2910=EDGE_LOOP('',(#12421,#12422,#12423,#12424));
#2911=EDGE_LOOP('',(#12425,#12426,#12427,#12428));
#2912=EDGE_LOOP('',(#12429,#12430,#12431,#12432));
#2913=EDGE_LOOP('',(#12433,#12434,#12435,#12436));
#2914=EDGE_LOOP('',(#12437,#12438,#12439,#12440));
#2915=EDGE_LOOP('',(#12441,#12442,#12443,#12444));
#2916=EDGE_LOOP('',(#12445,#12446,#12447,#12448));
#2917=EDGE_LOOP('',(#12449,#12450,#12451,#12452));
#2918=EDGE_LOOP('',(#12453,#12454,#12455,#12456));
#2919=EDGE_LOOP('',(#12457,#12458,#12459,#12460));
#2920=EDGE_LOOP('',(#12461,#12462,#12463,#12464));
#2921=EDGE_LOOP('',(#12465,#12466,#12467,#12468,#12469,#12470,#12471,#12472,
#12473,#12474,#12475,#12476,#12477,#12478,#12479,#12480,#12481,#12482,#12483,
#12484,#12485,#12486,#12487,#12488,#12489,#12490,#12491,#12492,#12493,#12494,
#12495,#12496,#12497,#12498,#12499,#12500,#12501,#12502,#12503,#12504,#12505,
#12506,#12507,#12508,#12509,#12510,#12511,#12512,#12513));
#2922=EDGE_LOOP('',(#12514,#12515,#12516,#12517,#12518));
#2923=EDGE_LOOP('',(#12519,#12520,#12521,#12522));
#2924=EDGE_LOOP('',(#12523,#12524,#12525,#12526,#12527,#12528,#12529,#12530,
#12531,#12532,#12533,#12534,#12535,#12536,#12537,#12538,#12539,#12540,#12541,
#12542,#12543,#12544,#12545,#12546,#12547,#12548,#12549,#12550,#12551,#12552,
#12553,#12554,#12555,#12556,#12557,#12558,#12559,#12560,#12561,#12562,#12563,
#12564,#12565,#12566,#12567,#12568,#12569,#12570,#12571));
#2925=EDGE_LOOP('',(#12572,#12573,#12574,#12575));
#2926=EDGE_LOOP('',(#12576));
#2927=EDGE_LOOP('',(#12577,#12578,#12579,#12580,#12581,#12582));
#2928=EDGE_LOOP('',(#12583,#12584,#12585,#12586,#12587,#12588,#12589,#12590,
#12591,#12592));
#2929=EDGE_LOOP('',(#12593,#12594,#12595,#12596));
#2930=EDGE_LOOP('',(#12597,#12598,#12599,#12600));
#2931=EDGE_LOOP('',(#12601,#12602,#12603,#12604));
#2932=EDGE_LOOP('',(#12605,#12606,#12607,#12608));
#2933=EDGE_LOOP('',(#12609,#12610,#12611,#12612));
#2934=EDGE_LOOP('',(#12613,#12614,#12615,#12616,#12617));
#2935=EDGE_LOOP('',(#12618));
#2936=EDGE_LOOP('',(#12619,#12620,#12621,#12622,#12623,#12624));
#2937=EDGE_LOOP('',(#12625,#12626,#12627,#12628));
#2938=EDGE_LOOP('',(#12629,#12630,#12631,#12632));
#2939=EDGE_LOOP('',(#12633,#12634,#12635,#12636));
#2940=EDGE_LOOP('',(#12637,#12638,#12639,#12640));
#2941=EDGE_LOOP('',(#12641,#12642,#12643,#12644));
#2942=EDGE_LOOP('',(#12645,#12646,#12647,#12648));
#2943=EDGE_LOOP('',(#12649,#12650,#12651,#12652));
#2944=EDGE_LOOP('',(#12653,#12654,#12655,#12656));
#2945=EDGE_LOOP('',(#12657,#12658,#12659,#12660));
#2946=EDGE_LOOP('',(#12661,#12662,#12663,#12664));
#2947=EDGE_LOOP('',(#12665,#12666,#12667,#12668));
#2948=EDGE_LOOP('',(#12669,#12670,#12671,#12672));
#2949=EDGE_LOOP('',(#12673,#12674,#12675,#12676));
#2950=EDGE_LOOP('',(#12677,#12678,#12679,#12680));
#2951=EDGE_LOOP('',(#12681,#12682,#12683,#12684));
#2952=EDGE_LOOP('',(#12685,#12686,#12687,#12688));
#2953=EDGE_LOOP('',(#12689,#12690,#12691,#12692));
#2954=EDGE_LOOP('',(#12693,#12694,#12695,#12696));
#2955=EDGE_LOOP('',(#12697,#12698,#12699,#12700));
#2956=EDGE_LOOP('',(#12701,#12702,#12703,#12704));
#2957=EDGE_LOOP('',(#12705,#12706,#12707,#12708));
#2958=EDGE_LOOP('',(#12709,#12710,#12711,#12712));
#2959=EDGE_LOOP('',(#12713,#12714,#12715,#12716));
#2960=EDGE_LOOP('',(#12717,#12718,#12719,#12720));
#2961=EDGE_LOOP('',(#12721,#12722,#12723,#12724));
#2962=EDGE_LOOP('',(#12725,#12726,#12727,#12728));
#2963=EDGE_LOOP('',(#12729,#12730,#12731,#12732));
#2964=EDGE_LOOP('',(#12733,#12734,#12735,#12736));
#2965=EDGE_LOOP('',(#12737,#12738,#12739,#12740));
#2966=EDGE_LOOP('',(#12741,#12742,#12743,#12744));
#2967=EDGE_LOOP('',(#12745,#12746,#12747,#12748));
#2968=EDGE_LOOP('',(#12749,#12750,#12751,#12752));
#2969=EDGE_LOOP('',(#12753,#12754,#12755,#12756));
#2970=EDGE_LOOP('',(#12757,#12758,#12759,#12760));
#2971=EDGE_LOOP('',(#12761,#12762,#12763,#12764));
#2972=EDGE_LOOP('',(#12765,#12766,#12767,#12768));
#2973=EDGE_LOOP('',(#12769,#12770,#12771,#12772));
#2974=EDGE_LOOP('',(#12773,#12774,#12775,#12776));
#2975=EDGE_LOOP('',(#12777,#12778,#12779,#12780));
#2976=EDGE_LOOP('',(#12781,#12782,#12783,#12784));
#2977=EDGE_LOOP('',(#12785,#12786,#12787,#12788));
#2978=EDGE_LOOP('',(#12789,#12790,#12791,#12792));
#2979=EDGE_LOOP('',(#12793,#12794,#12795,#12796));
#2980=EDGE_LOOP('',(#12797,#12798,#12799,#12800));
#2981=EDGE_LOOP('',(#12801,#12802,#12803,#12804));
#2982=EDGE_LOOP('',(#12805,#12806,#12807,#12808));
#2983=EDGE_LOOP('',(#12809,#12810,#12811,#12812));
#2984=EDGE_LOOP('',(#12813,#12814,#12815,#12816));
#2985=EDGE_LOOP('',(#12817,#12818,#12819,#12820));
#2986=EDGE_LOOP('',(#12821,#12822,#12823,#12824));
#2987=EDGE_LOOP('',(#12825,#12826,#12827,#12828));
#2988=EDGE_LOOP('',(#12829,#12830,#12831,#12832));
#2989=EDGE_LOOP('',(#12833,#12834,#12835,#12836));
#2990=EDGE_LOOP('',(#12837,#12838,#12839,#12840));
#2991=EDGE_LOOP('',(#12841,#12842,#12843,#12844));
#2992=EDGE_LOOP('',(#12845,#12846,#12847,#12848));
#2993=EDGE_LOOP('',(#12849,#12850,#12851,#12852));
#2994=EDGE_LOOP('',(#12853,#12854,#12855,#12856,#12857,#12858,#12859,#12860,
#12861,#12862,#12863,#12864,#12865,#12866,#12867,#12868,#12869,#12870,#12871,
#12872,#12873,#12874,#12875,#12876,#12877,#12878,#12879,#12880,#12881,#12882,
#12883,#12884,#12885,#12886,#12887,#12888,#12889,#12890,#12891,#12892,#12893,
#12894,#12895,#12896,#12897,#12898,#12899,#12900,#12901,#12902,#12903,#12904,
#12905,#12906,#12907,#12908,#12909,#12910,#12911,#12912));
#2995=EDGE_LOOP('',(#12913,#12914,#12915,#12916,#12917));
#2996=EDGE_LOOP('',(#12918,#12919,#12920,#12921));
#2997=EDGE_LOOP('',(#12922,#12923,#12924,#12925,#12926,#12927,#12928,#12929,
#12930,#12931,#12932,#12933,#12934,#12935,#12936,#12937,#12938,#12939,#12940,
#12941,#12942,#12943,#12944,#12945,#12946,#12947,#12948,#12949,#12950,#12951,
#12952,#12953,#12954,#12955,#12956,#12957,#12958,#12959,#12960,#12961,#12962,
#12963,#12964,#12965,#12966,#12967,#12968,#12969,#12970,#12971,#12972,#12973,
#12974,#12975,#12976,#12977,#12978,#12979,#12980,#12981));
#2998=EDGE_LOOP('',(#12982,#12983,#12984));
#2999=EDGE_LOOP('',(#12985,#12986,#12987,#12988));
#3000=EDGE_LOOP('',(#12989,#12990,#12991,#12992));
#3001=EDGE_LOOP('',(#12993,#12994,#12995,#12996));
#3002=EDGE_LOOP('',(#12997,#12998,#12999,#13000));
#3003=EDGE_LOOP('',(#13001,#13002,#13003,#13004));
#3004=EDGE_LOOP('',(#13005,#13006,#13007,#13008));
#3005=EDGE_LOOP('',(#13009,#13010,#13011,#13012,#13013,#13014));
#3006=EDGE_LOOP('',(#13015));
#3007=EDGE_LOOP('',(#13016));
#3008=EDGE_LOOP('',(#13017,#13018,#13019,#13020,#13021,#13022));
#3009=EDGE_LOOP('',(#13023,#13024,#13025,#13026));
#3010=EDGE_LOOP('',(#13027));
#3011=EDGE_LOOP('',(#13028,#13029,#13030,#13031));
#3012=EDGE_LOOP('',(#13032,#13033,#13034,#13035,#13036));
#3013=EDGE_LOOP('',(#13037,#13038,#13039,#13040,#13041,#13042,#13043,#13044,
#13045,#13046));
#3014=EDGE_LOOP('',(#13047,#13048,#13049,#13050,#13051));
#3015=EDGE_LOOP('',(#13052,#13053,#13054,#13055,#13056));
#3016=EDGE_LOOP('',(#13057));
#3017=EDGE_LOOP('',(#13058));
#3018=EDGE_LOOP('',(#13059,#13060,#13061,#13062));
#3019=EDGE_LOOP('',(#13063));
#3020=EDGE_LOOP('',(#13064));
#3021=EDGE_LOOP('',(#13065,#13066,#13067,#13068));
#3022=EDGE_LOOP('',(#13069,#13070,#13071,#13072));
#3023=EDGE_LOOP('',(#13073,#13074,#13075,#13076));
#3024=EDGE_LOOP('',(#13077,#13078,#13079,#13080,#13081,#13082,#13083,#13084,
#13085,#13086,#13087,#13088,#13089,#13090,#13091,#13092));
#3025=EDGE_LOOP('',(#13093,#13094,#13095,#13096));
#3026=EDGE_LOOP('',(#13097,#13098,#13099,#13100));
#3027=EDGE_LOOP('',(#13101));
#3028=EDGE_LOOP('',(#13102));
#3029=EDGE_LOOP('',(#13103,#13104,#13105,#13106));
#3030=EDGE_LOOP('',(#13107));
#3031=EDGE_LOOP('',(#13108));
#3032=EDGE_LOOP('',(#13109,#13110,#13111,#13112));
#3033=EDGE_LOOP('',(#13113,#13114,#13115,#13116));
#3034=EDGE_LOOP('',(#13117,#13118,#13119,#13120,#13121,#13122,#13123,#13124,
#13125,#13126,#13127,#13128,#13129,#13130,#13131,#13132));
#3035=EDGE_LOOP('',(#13133,#13134,#13135,#13136));
#3036=EDGE_LOOP('',(#13137,#13138,#13139,#13140,#13141,#13142));
#3037=EDGE_LOOP('',(#13143,#13144,#13145,#13146));
#3038=EDGE_LOOP('',(#13147,#13148,#13149,#13150));
#3039=EDGE_LOOP('',(#13151,#13152,#13153,#13154));
#3040=EDGE_LOOP('',(#13155,#13156,#13157,#13158));
#3041=EDGE_LOOP('',(#13159,#13160,#13161,#13162));
#3042=EDGE_LOOP('',(#13163,#13164,#13165,#13166));
#3043=EDGE_LOOP('',(#13167,#13168,#13169,#13170));
#3044=EDGE_LOOP('',(#13171,#13172,#13173,#13174));
#3045=EDGE_LOOP('',(#13175,#13176,#13177,#13178));
#3046=EDGE_LOOP('',(#13179,#13180,#13181,#13182));
#3047=EDGE_LOOP('',(#13183,#13184,#13185,#13186));
#3048=EDGE_LOOP('',(#13187,#13188,#13189,#13190));
#3049=EDGE_LOOP('',(#13191,#13192,#13193,#13194));
#3050=EDGE_LOOP('',(#13195,#13196,#13197,#13198));
#3051=EDGE_LOOP('',(#13199,#13200,#13201,#13202));
#3052=EDGE_LOOP('',(#13203,#13204,#13205,#13206));
#3053=EDGE_LOOP('',(#13207,#13208,#13209,#13210));
#3054=EDGE_LOOP('',(#13211,#13212,#13213,#13214));
#3055=EDGE_LOOP('',(#13215,#13216,#13217,#13218));
#3056=EDGE_LOOP('',(#13219,#13220,#13221,#13222));
#3057=EDGE_LOOP('',(#13223,#13224,#13225,#13226));
#3058=EDGE_LOOP('',(#13227,#13228,#13229,#13230));
#3059=EDGE_LOOP('',(#13231,#13232,#13233,#13234));
#3060=EDGE_LOOP('',(#13235,#13236,#13237,#13238,#13239));
#3061=EDGE_LOOP('',(#13240,#13241,#13242,#13243));
#3062=EDGE_LOOP('',(#13244,#13245,#13246,#13247));
#3063=EDGE_LOOP('',(#13248,#13249,#13250,#13251));
#3064=EDGE_LOOP('',(#13252,#13253,#13254,#13255));
#3065=EDGE_LOOP('',(#13256,#13257,#13258,#13259));
#3066=EDGE_LOOP('',(#13260,#13261,#13262,#13263));
#3067=EDGE_LOOP('',(#13264,#13265,#13266,#13267));
#3068=EDGE_LOOP('',(#13268,#13269,#13270,#13271));
#3069=EDGE_LOOP('',(#13272,#13273,#13274,#13275));
#3070=EDGE_LOOP('',(#13276,#13277,#13278,#13279));
#3071=EDGE_LOOP('',(#13280,#13281,#13282,#13283));
#3072=EDGE_LOOP('',(#13284,#13285,#13286,#13287));
#3073=EDGE_LOOP('',(#13288,#13289,#13290,#13291));
#3074=EDGE_LOOP('',(#13292,#13293,#13294,#13295));
#3075=EDGE_LOOP('',(#13296,#13297,#13298,#13299));
#3076=EDGE_LOOP('',(#13300,#13301,#13302,#13303));
#3077=EDGE_LOOP('',(#13304,#13305,#13306,#13307));
#3078=EDGE_LOOP('',(#13308,#13309,#13310,#13311,#13312,#13313,#13314,#13315,
#13316,#13317,#13318,#13319,#13320,#13321,#13322,#13323,#13324,#13325,#13326,
#13327,#13328,#13329,#13330,#13331,#13332,#13333,#13334,#13335,#13336,#13337,
#13338,#13339,#13340,#13341,#13342,#13343,#13344,#13345,#13346));
#3079=EDGE_LOOP('',(#13347,#13348,#13349,#13350,#13351));
#3080=EDGE_LOOP('',(#13352,#13353,#13354,#13355));
#3081=EDGE_LOOP('',(#13356,#13357,#13358,#13359,#13360,#13361,#13362,#13363,
#13364,#13365,#13366,#13367,#13368,#13369,#13370,#13371,#13372,#13373,#13374,
#13375,#13376,#13377,#13378,#13379,#13380,#13381,#13382,#13383,#13384,#13385,
#13386,#13387,#13388,#13389,#13390,#13391,#13392,#13393));
#3082=EDGE_LOOP('',(#13394,#13395,#13396));
#3083=EDGE_LOOP('',(#13397,#13398,#13399,#13400));
#3084=EDGE_LOOP('',(#13401,#13402,#13403,#13404));
#3085=EDGE_LOOP('',(#13405,#13406,#13407,#13408));
#3086=EDGE_LOOP('',(#13409,#13410,#13411,#13412));
#3087=EDGE_LOOP('',(#13413,#13414,#13415,#13416));
#3088=EDGE_LOOP('',(#13417,#13418,#13419,#13420));
#3089=EDGE_LOOP('',(#13421,#13422,#13423,#13424,#13425,#13426));
#3090=EDGE_LOOP('',(#13427));
#3091=EDGE_LOOP('',(#13428));
#3092=EDGE_LOOP('',(#13429,#13430,#13431,#13432,#13433,#13434));
#3093=EDGE_LOOP('',(#13435,#13436,#13437));
#3094=EDGE_LOOP('',(#13438));
#3095=EDGE_LOOP('',(#13439,#13440,#13441,#13442,#13443));
#3096=EDGE_LOOP('',(#13444,#13445,#13446,#13447,#13448));
#3097=EDGE_LOOP('',(#13449,#13450,#13451,#13452,#13453,#13454,#13455,#13456,
#13457,#13458));
#3098=(
BOUNDED_CURVE()
B_SPLINE_CURVE(2,(#19759,#19760,#19761),.UNSPECIFIED.,.F.,.F.)
B_SPLINE_CURVE_WITH_KNOTS((3,3),(0.0434191036447886,0.0876516150043351),
 .UNSPECIFIED.)
CURVE()
GEOMETRIC_REPRESENTATION_ITEM()
RATIONAL_B_SPLINE_CURVE((1.00007900493244,1.00007974496639,1.))
REPRESENTATION_ITEM('')
);
#3099=(
BOUNDED_CURVE()
B_SPLINE_CURVE(2,(#19764,#19765,#19766),.UNSPECIFIED.,.F.,.F.)
B_SPLINE_CURVE_WITH_KNOTS((3,3),(0.,0.0442325113595662),.UNSPECIFIED.)
CURVE()
GEOMETRIC_REPRESENTATION_ITEM()
RATIONAL_B_SPLINE_CURVE((1.,1.00007974496581,1.00007900493187))
REPRESENTATION_ITEM('')
);
#3100=(
BOUNDED_CURVE()
B_SPLINE_CURVE(2,(#19769,#19770,#19771),.UNSPECIFIED.,.F.,.F.)
B_SPLINE_CURVE_WITH_KNOTS((3,3),(0.0429017134859095,0.085594459730905),
 .UNSPECIFIED.)
CURVE()
GEOMETRIC_REPRESENTATION_ITEM()
RATIONAL_B_SPLINE_CURVE((1.,1.,1.))
REPRESENTATION_ITEM('')
);
#3101=(
BOUNDED_CURVE()
B_SPLINE_CURVE(2,(#19781,#19782,#19783),.UNSPECIFIED.,.F.,.F.)
B_SPLINE_CURVE_WITH_KNOTS((3,3),(0.0434191036447867,0.0876516150043353),
 .UNSPECIFIED.)
CURVE()
GEOMETRIC_REPRESENTATION_ITEM()
RATIONAL_B_SPLINE_CURVE((1.00007900493282,1.00007974496678,1.))
REPRESENTATION_ITEM('')
);
#3102=(
BOUNDED_CURVE()
B_SPLINE_CURVE(2,(#19785,#19786,#19787),.UNSPECIFIED.,.F.,.F.)
B_SPLINE_CURVE_WITH_KNOTS((3,3),(0.,0.0426927462450535),.UNSPECIFIED.)
CURVE()
GEOMETRIC_REPRESENTATION_ITEM()
RATIONAL_B_SPLINE_CURVE((1.,1.,1.))
REPRESENTATION_ITEM('')
);
#3103=(
BOUNDED_CURVE()
B_SPLINE_CURVE(2,(#19819,#19820,#19821),.UNSPECIFIED.,.F.,.F.)
B_SPLINE_CURVE_WITH_KNOTS((3,3),(0.,0.0785138217700896),.UNSPECIFIED.)
CURVE()
GEOMETRIC_REPRESENTATION_ITEM()
RATIONAL_B_SPLINE_CURVE((1.,1.,1.))
REPRESENTATION_ITEM('')
);
#3104=(
BOUNDED_CURVE()
B_SPLINE_CURVE(2,(#19828,#19829,#19830),.UNSPECIFIED.,.F.,.F.)
B_SPLINE_CURVE_WITH_KNOTS((3,3),(0.,0.0426927462450536),.UNSPECIFIED.)
CURVE()
GEOMETRIC_REPRESENTATION_ITEM()
RATIONAL_B_SPLINE_CURVE((1.,1.,1.))
REPRESENTATION_ITEM('')
);
#3105=(
BOUNDED_CURVE()
B_SPLINE_CURVE(2,(#19837,#19838,#19839),.UNSPECIFIED.,.F.,.F.)
B_SPLINE_CURVE_WITH_KNOTS((3,3),(0.,0.0785138217700896),.UNSPECIFIED.)
CURVE()
GEOMETRIC_REPRESENTATION_ITEM()
RATIONAL_B_SPLINE_CURVE((1.,1.,1.))
REPRESENTATION_ITEM('')
);
#3106=(
BOUNDED_CURVE()
B_SPLINE_CURVE(2,(#19872,#19873,#19874),.UNSPECIFIED.,.F.,.F.)
B_SPLINE_CURVE_WITH_KNOTS((3,3),(0.0686220150831262,0.071456332389423),
 .UNSPECIFIED.)
CURVE()
GEOMETRIC_REPRESENTATION_ITEM()
RATIONAL_B_SPLINE_CURVE((1.00000280409598,1.00000145995723,1.))
REPRESENTATION_ITEM('')
);
#3107=(
BOUNDED_CURVE()
B_SPLINE_CURVE(2,(#19877,#19878,#19879),.UNSPECIFIED.,.F.,.F.)
B_SPLINE_CURVE_WITH_KNOTS((3,3),(0.,0.00283431730629652),.UNSPECIFIED.)
CURVE()
GEOMETRIC_REPRESENTATION_ITEM()
RATIONAL_B_SPLINE_CURVE((1.,1.00000145995723,1.00000280409598))
REPRESENTATION_ITEM('')
);
#3108=(
BOUNDED_CURVE()
B_SPLINE_CURVE(2,(#19889,#19890,#19891),.UNSPECIFIED.,.F.,.F.)
B_SPLINE_CURVE_WITH_KNOTS((3,3),(0.,0.0442325113595461),.UNSPECIFIED.)
CURVE()
GEOMETRIC_REPRESENTATION_ITEM()
RATIONAL_B_SPLINE_CURVE((1.,1.00007974496639,1.00007900493244))
REPRESENTATION_ITEM('')
);
#3109=(
BOUNDED_CURVE()
B_SPLINE_CURVE(2,(#19909,#19910,#19911),.UNSPECIFIED.,.F.,.F.)
B_SPLINE_CURVE_WITH_KNOTS((3,3),(0.0429017134859048,0.0855944597309048),
 .UNSPECIFIED.)
CURVE()
GEOMETRIC_REPRESENTATION_ITEM()
RATIONAL_B_SPLINE_CURVE((1.,1.,1.))
REPRESENTATION_ITEM('')
);
#3110=(
BOUNDED_CURVE()
B_SPLINE_CURVE(2,(#19915,#19916,#19917),.UNSPECIFIED.,.F.,.F.)
B_SPLINE_CURVE_WITH_KNOTS((3,3),(0.,0.0785138217700896),.UNSPECIFIED.)
CURVE()
GEOMETRIC_REPRESENTATION_ITEM()
RATIONAL_B_SPLINE_CURVE((1.,1.,1.))
REPRESENTATION_ITEM('')
);
#3111=(
BOUNDED_CURVE()
B_SPLINE_CURVE(2,(#19945,#19946,#19947),.UNSPECIFIED.,.F.,.F.)
B_SPLINE_CURVE_WITH_KNOTS((3,3),(0.,0.0785138217700896),.UNSPECIFIED.)
CURVE()
GEOMETRIC_REPRESENTATION_ITEM()
RATIONAL_B_SPLINE_CURVE((1.,1.,1.))
REPRESENTATION_ITEM('')
);
#3112=(
BOUNDED_CURVE()
B_SPLINE_CURVE(2,(#19956,#19957,#19958),.UNSPECIFIED.,.F.,.F.)
B_SPLINE_CURVE_WITH_KNOTS((3,3),(0.0686220150831262,0.071456332389423),
 .UNSPECIFIED.)
CURVE()
GEOMETRIC_REPRESENTATION_ITEM()
RATIONAL_B_SPLINE_CURVE((1.00000280409598,1.00000145995723,1.))
REPRESENTATION_ITEM('')
);
#3113=(
BOUNDED_CURVE()
B_SPLINE_CURVE(2,(#19962,#19963,#19964),.UNSPECIFIED.,.F.,.F.)
B_SPLINE_CURVE_WITH_KNOTS((3,3),(0.,0.00283431730629652),.UNSPECIFIED.)
CURVE()
GEOMETRIC_REPRESENTATION_ITEM()
RATIONAL_B_SPLINE_CURVE((1.,1.00000145995723,1.00000280409598))
REPRESENTATION_ITEM('')
);
#3114=(
BOUNDED_CURVE()
B_SPLINE_CURVE(2,(#20022,#20023,#20024),.UNSPECIFIED.,.F.,.F.)
B_SPLINE_CURVE_WITH_KNOTS((3,3),(0.,0.0711434865298028),.UNSPECIFIED.)
CURVE()
GEOMETRIC_REPRESENTATION_ITEM()
RATIONAL_B_SPLINE_CURVE((1.,1.,1.))
REPRESENTATION_ITEM('')
);
#3115=(
BOUNDED_CURVE()
B_SPLINE_CURVE(2,(#20032,#20033,#20034),.UNSPECIFIED.,.F.,.F.)
B_SPLINE_CURVE_WITH_KNOTS((3,3),(0.0811630519003425,0.084492689542221),
 .UNSPECIFIED.)
CURVE()
GEOMETRIC_REPRESENTATION_ITEM()
RATIONAL_B_SPLINE_CURVE((1.0000049607761,1.00000258214363,1.))
REPRESENTATION_ITEM('')
);
#3116=(
BOUNDED_CURVE()
B_SPLINE_CURVE(2,(#20038,#20039,#20040),.UNSPECIFIED.,.F.,.F.)
B_SPLINE_CURVE_WITH_KNOTS((3,3),(0.,0.00332963764187841),.UNSPECIFIED.)
CURVE()
GEOMETRIC_REPRESENTATION_ITEM()
RATIONAL_B_SPLINE_CURVE((1.,1.00000258214363,1.0000049607761))
REPRESENTATION_ITEM('')
);
#3117=(
BOUNDED_CURVE()
B_SPLINE_CURVE(2,(#20175,#20176,#20177),.UNSPECIFIED.,.F.,.F.)
B_SPLINE_CURVE_WITH_KNOTS((3,3),(0.0429017134859085,0.0855944597309053),
 .UNSPECIFIED.)
CURVE()
GEOMETRIC_REPRESENTATION_ITEM()
RATIONAL_B_SPLINE_CURVE((1.,1.,1.))
REPRESENTATION_ITEM('')
);
#3118=(
BOUNDED_CURVE()
B_SPLINE_CURVE(2,(#20183,#20184,#20185),.UNSPECIFIED.,.F.,.F.)
B_SPLINE_CURVE_WITH_KNOTS((3,3),(0.,0.0711434865298028),.UNSPECIFIED.)
CURVE()
GEOMETRIC_REPRESENTATION_ITEM()
RATIONAL_B_SPLINE_CURVE((1.,1.,1.))
REPRESENTATION_ITEM('')
);
#3119=(
BOUNDED_CURVE()
B_SPLINE_CURVE(2,(#20192,#20193,#20194),.UNSPECIFIED.,.F.,.F.)
B_SPLINE_CURVE_WITH_KNOTS((3,3),(0.081163051900335,0.0844926895422209),
 .UNSPECIFIED.)
CURVE()
GEOMETRIC_REPRESENTATION_ITEM()
RATIONAL_B_SPLINE_CURVE((1.00000496077593,1.00000258214354,1.))
REPRESENTATION_ITEM('')
);
#3120=(
BOUNDED_CURVE()
B_SPLINE_CURVE(2,(#20197,#20198,#20199),.UNSPECIFIED.,.F.,.F.)
B_SPLINE_CURVE_WITH_KNOTS((3,3),(0.,0.00332963764188661),.UNSPECIFIED.)
CURVE()
GEOMETRIC_REPRESENTATION_ITEM()
RATIONAL_B_SPLINE_CURVE((1.,1.00000258214354,1.00000496077593))
REPRESENTATION_ITEM('')
);
#3121=(
BOUNDED_CURVE()
B_SPLINE_CURVE(2,(#20231,#20232,#20233),.UNSPECIFIED.,.F.,.F.)
B_SPLINE_CURVE_WITH_KNOTS((3,3),(0.,0.0426927462449967),.UNSPECIFIED.)
CURVE()
GEOMETRIC_REPRESENTATION_ITEM()
RATIONAL_B_SPLINE_CURVE((1.,1.,1.))
REPRESENTATION_ITEM('')
);
#3122=(
BOUNDED_CURVE()
B_SPLINE_CURVE(2,(#20250,#20251,#20252),.UNSPECIFIED.,.F.,.F.)
B_SPLINE_CURVE_WITH_KNOTS((3,3),(0.0429017134858602,0.0855944597309048),
 .UNSPECIFIED.)
CURVE()
GEOMETRIC_REPRESENTATION_ITEM()
RATIONAL_B_SPLINE_CURVE((1.,1.,1.))
REPRESENTATION_ITEM('')
);
#3123=(
BOUNDED_CURVE()
B_SPLINE_CURVE(2,(#20259,#20260,#20261),.UNSPECIFIED.,.F.,.F.)
B_SPLINE_CURVE_WITH_KNOTS((3,3),(0.043419103644769,0.0876516150043356),
 .UNSPECIFIED.)
CURVE()
GEOMETRIC_REPRESENTATION_ITEM()
RATIONAL_B_SPLINE_CURVE((1.00007900493187,1.00007974496581,1.))
REPRESENTATION_ITEM('')
);
#3124=(
BOUNDED_CURVE()
B_SPLINE_CURVE(2,(#20264,#20265,#20266),.UNSPECIFIED.,.F.,.F.)
B_SPLINE_CURVE_WITH_KNOTS((3,3),(0.,0.044232511359626),.UNSPECIFIED.)
CURVE()
GEOMETRIC_REPRESENTATION_ITEM()
RATIONAL_B_SPLINE_CURVE((1.,1.00007974496639,1.00007900493244))
REPRESENTATION_ITEM('')
);
#3125=(
BOUNDED_CURVE()
B_SPLINE_CURVE(2,(#20309,#20310,#20311),.UNSPECIFIED.,.F.,.F.)
B_SPLINE_CURVE_WITH_KNOTS((3,3),(0.,0.0711434865298029),.UNSPECIFIED.)
CURVE()
GEOMETRIC_REPRESENTATION_ITEM()
RATIONAL_B_SPLINE_CURVE((1.,1.,1.))
REPRESENTATION_ITEM('')
);
#3126=(
BOUNDED_CURVE()
B_SPLINE_CURVE(2,(#20335,#20336,#20337),.UNSPECIFIED.,.F.,.F.)
B_SPLINE_CURVE_WITH_KNOTS((3,3),(0.,0.0711434865298029),.UNSPECIFIED.)
CURVE()
GEOMETRIC_REPRESENTATION_ITEM()
RATIONAL_B_SPLINE_CURVE((1.,1.,1.))
REPRESENTATION_ITEM('')
);
#3127=(
BOUNDED_CURVE()
B_SPLINE_CURVE(2,(#20340,#20341,#20342),.UNSPECIFIED.,.F.,.F.)
B_SPLINE_CURVE_WITH_KNOTS((3,3),(0.,0.0426927462450447),.UNSPECIFIED.)
CURVE()
GEOMETRIC_REPRESENTATION_ITEM()
RATIONAL_B_SPLINE_CURVE((1.,1.,1.))
REPRESENTATION_ITEM('')
);
#3128=(
BOUNDED_CURVE()
B_SPLINE_CURVE(2,(#20354,#20355,#20356),.UNSPECIFIED.,.F.,.F.)
B_SPLINE_CURVE_WITH_KNOTS((3,3),(0.0434191036447888,0.0876516150043351),
 .UNSPECIFIED.)
CURVE()
GEOMETRIC_REPRESENTATION_ITEM()
RATIONAL_B_SPLINE_CURVE((1.00007900493244,1.00007974496639,1.))
REPRESENTATION_ITEM('')
);
#3129=(
BOUNDED_CURVE()
B_SPLINE_CURVE(2,(#20361,#20362,#20363),.UNSPECIFIED.,.F.,.F.)
B_SPLINE_CURVE_WITH_KNOTS((3,3),(0.,0.0442325113596284),.UNSPECIFIED.)
CURVE()
GEOMETRIC_REPRESENTATION_ITEM()
RATIONAL_B_SPLINE_CURVE((1.,1.00007974496678,1.00007900493282))
REPRESENTATION_ITEM('')
);
#3130=(
BOUNDED_CURVE()
B_SPLINE_CURVE(2,(#20405,#20406,#20407),.UNSPECIFIED.,.F.,.F.)
B_SPLINE_CURVE_WITH_KNOTS((3,3),(-3.26709460117384,-3.09375460254933),
 .UNSPECIFIED.)
CURVE()
GEOMETRIC_REPRESENTATION_ITEM()
RATIONAL_B_SPLINE_CURVE((1.22511255627814,1.2314549978879,1.23649074068738))
REPRESENTATION_ITEM('')
);
#3131=(
BOUNDED_CURVE()
B_SPLINE_CURVE(2,(#20408,#20409,#20410),.UNSPECIFIED.,.F.,.F.)
B_SPLINE_CURVE_WITH_KNOTS((3,3),(-1.75772269823236,-1.58438269960785),
 .UNSPECIFIED.)
CURVE()
GEOMETRIC_REPRESENTATION_ITEM()
RATIONAL_B_SPLINE_CURVE((1.23649074068738,1.2314549978879,1.22511255627814))
REPRESENTATION_ITEM('')
);
#3132=(
BOUNDED_CURVE()
B_SPLINE_CURVE(2,(#20413,#20414,#20415),.UNSPECIFIED.,.F.,.F.)
B_SPLINE_CURVE_WITH_KNOTS((3,3),(-1.75772269823236,-1.58438269960785),
 .UNSPECIFIED.)
CURVE()
GEOMETRIC_REPRESENTATION_ITEM()
RATIONAL_B_SPLINE_CURVE((1.23649074068738,1.2314549978879,1.22511255627814))
REPRESENTATION_ITEM('')
);
#3133=(
BOUNDED_CURVE()
B_SPLINE_CURVE(2,(#20418,#20419,#20420),.UNSPECIFIED.,.F.,.F.)
B_SPLINE_CURVE_WITH_KNOTS((3,3),(-3.26709460117384,-3.09375460254933),
 .UNSPECIFIED.)
CURVE()
GEOMETRIC_REPRESENTATION_ITEM()
RATIONAL_B_SPLINE_CURVE((1.22511255627814,1.2314549978879,1.23649074068738))
REPRESENTATION_ITEM('')
);
#3134=(
BOUNDED_CURVE()
B_SPLINE_CURVE(2,(#20466,#20467,#20468),.UNSPECIFIED.,.F.,.F.)
B_SPLINE_CURVE_WITH_KNOTS((3,3),(-0.360391606906832,-0.356059784727892),
 .UNSPECIFIED.)
CURVE()
GEOMETRIC_REPRESENTATION_ITEM()
RATIONAL_B_SPLINE_CURVE((1.0105812122411,1.01053365079744,1.01048570399065))
REPRESENTATION_ITEM('')
);
#3135=(
BOUNDED_CURVE()
B_SPLINE_CURVE(2,(#20470,#20471,#20472),.UNSPECIFIED.,.F.,.F.)
B_SPLINE_CURVE_WITH_KNOTS((3,3),(-1.43398872568548,-1.42965690350654),
 .UNSPECIFIED.)
CURVE()
GEOMETRIC_REPRESENTATION_ITEM()
RATIONAL_B_SPLINE_CURVE((1.01048570399065,1.01053365079744,1.0105812122411))
REPRESENTATION_ITEM('')
);
#3136=(
BOUNDED_CURVE()
B_SPLINE_CURVE(2,(#20476,#20477,#20478),.UNSPECIFIED.,.F.,.F.)
B_SPLINE_CURVE_WITH_KNOTS((3,3),(-1.43398872568546,-1.42965690350652),
 .UNSPECIFIED.)
CURVE()
GEOMETRIC_REPRESENTATION_ITEM()
RATIONAL_B_SPLINE_CURVE((1.01048570399063,1.01053365079743,1.01058121224108))
REPRESENTATION_ITEM('')
);
#3137=(
BOUNDED_CURVE()
B_SPLINE_CURVE(2,(#20481,#20482,#20483),.UNSPECIFIED.,.F.,.F.)
B_SPLINE_CURVE_WITH_KNOTS((3,3),(-0.360391606906842,-0.356059784727902),
 .UNSPECIFIED.)
CURVE()
GEOMETRIC_REPRESENTATION_ITEM()
RATIONAL_B_SPLINE_CURVE((1.01058121224108,1.01053365079743,1.01048570399063))
REPRESENTATION_ITEM('')
);
#3138=(
BOUNDED_CURVE()
B_SPLINE_CURVE(2,(#26226,#26227,#26228),.UNSPECIFIED.,.F.,.F.)
B_SPLINE_CURVE_WITH_KNOTS((3,3),(0.136653338911782,0.195398016960284),
 .UNSPECIFIED.)
CURVE()
GEOMETRIC_REPRESENTATION_ITEM()
RATIONAL_B_SPLINE_CURVE((1.00492385476096,1.00359200155149,1.00020515445013))
REPRESENTATION_ITEM('')
);
#3139=(
BOUNDED_CURVE()
B_SPLINE_CURVE(2,(#26385,#26386,#26387),.UNSPECIFIED.,.F.,.F.)
B_SPLINE_CURVE_WITH_KNOTS((3,3),(0.0017631420801792,0.0605078201286812),
 .UNSPECIFIED.)
CURVE()
GEOMETRIC_REPRESENTATION_ITEM()
RATIONAL_B_SPLINE_CURVE((1.00020515445013,1.00359200155149,1.00492385476096))
REPRESENTATION_ITEM('')
);
#3140=(
BOUNDED_CURVE()
B_SPLINE_CURVE(2,(#26389,#26390,#26391),.UNSPECIFIED.,.F.,.F.)
B_SPLINE_CURVE_WITH_KNOTS((3,3),(0.136653338911781,0.195398016960283),
 .UNSPECIFIED.)
CURVE()
GEOMETRIC_REPRESENTATION_ITEM()
RATIONAL_B_SPLINE_CURVE((1.00492385476097,1.0035920015515,1.00020515445013))
REPRESENTATION_ITEM('')
);
#3141=(
BOUNDED_CURVE()
B_SPLINE_CURVE(2,(#26403,#26404,#26405),.UNSPECIFIED.,.F.,.F.)
B_SPLINE_CURVE_WITH_KNOTS((3,3),(0.00176314208017943,0.060507820128681),
 .UNSPECIFIED.)
CURVE()
GEOMETRIC_REPRESENTATION_ITEM()
RATIONAL_B_SPLINE_CURVE((1.00020515445013,1.00359200155151,1.00492385476097))
REPRESENTATION_ITEM('')
);
#3142=(
BOUNDED_CURVE()
B_SPLINE_CURVE(2,(#26407,#26408,#26409),.UNSPECIFIED.,.F.,.F.)
B_SPLINE_CURVE_WITH_KNOTS((3,3),(0.136653338911775,0.195398016960278),
 .UNSPECIFIED.)
CURVE()
GEOMETRIC_REPRESENTATION_ITEM()
RATIONAL_B_SPLINE_CURVE((1.00492385476094,1.00359200155148,1.00020515445012))
REPRESENTATION_ITEM('')
);
#3143=(
BOUNDED_CURVE()
B_SPLINE_CURVE(2,(#26421,#26422,#26423),.UNSPECIFIED.,.F.,.F.)
B_SPLINE_CURVE_WITH_KNOTS((3,3),(0.00176314208017901,0.0605078201286807),
 .UNSPECIFIED.)
CURVE()
GEOMETRIC_REPRESENTATION_ITEM()
RATIONAL_B_SPLINE_CURVE((1.00020515445013,1.0035920015515,1.00492385476096))
REPRESENTATION_ITEM('')
);
#3144=(
BOUNDED_CURVE()
B_SPLINE_CURVE(2,(#26425,#26426,#26427),.UNSPECIFIED.,.F.,.F.)
B_SPLINE_CURVE_WITH_KNOTS((3,3),(0.136653338911781,0.195398016960283),
 .UNSPECIFIED.)
CURVE()
GEOMETRIC_REPRESENTATION_ITEM()
RATIONAL_B_SPLINE_CURVE((1.00492385476095,1.00359200155149,1.00020515445012))
REPRESENTATION_ITEM('')
);
#3145=(
BOUNDED_CURVE()
B_SPLINE_CURVE(2,(#26439,#26440,#26441),.UNSPECIFIED.,.F.,.F.)
B_SPLINE_CURVE_WITH_KNOTS((3,3),(0.00176314208017882,0.0605078201286799),
 .UNSPECIFIED.)
CURVE()
GEOMETRIC_REPRESENTATION_ITEM()
RATIONAL_B_SPLINE_CURVE((1.00020515445013,1.00359200155151,1.00492385476098))
REPRESENTATION_ITEM('')
);
#3146=(
BOUNDED_CURVE()
B_SPLINE_CURVE(2,(#26443,#26444,#26445),.UNSPECIFIED.,.F.,.F.)
B_SPLINE_CURVE_WITH_KNOTS((3,3),(0.136653338911781,0.195398016960283),
 .UNSPECIFIED.)
CURVE()
GEOMETRIC_REPRESENTATION_ITEM()
RATIONAL_B_SPLINE_CURVE((1.00492385476096,1.0035920015515,1.00020515445013))
REPRESENTATION_ITEM('')
);
#3147=(
BOUNDED_CURVE()
B_SPLINE_CURVE(2,(#26457,#26458,#26459),.UNSPECIFIED.,.F.,.F.)
B_SPLINE_CURVE_WITH_KNOTS((3,3),(0.0017631420801791,0.0605078201286811),
 .UNSPECIFIED.)
CURVE()
GEOMETRIC_REPRESENTATION_ITEM()
RATIONAL_B_SPLINE_CURVE((1.00020515445012,1.00359200155149,1.00492385476095))
REPRESENTATION_ITEM('')
);
#3148=(
BOUNDED_CURVE()
B_SPLINE_CURVE(2,(#26461,#26462,#26463),.UNSPECIFIED.,.F.,.F.)
B_SPLINE_CURVE_WITH_KNOTS((3,3),(0.136653338911783,0.195398016960284),
 .UNSPECIFIED.)
CURVE()
GEOMETRIC_REPRESENTATION_ITEM()
RATIONAL_B_SPLINE_CURVE((1.00492385476097,1.0035920015515,1.00020515445013))
REPRESENTATION_ITEM('')
);
#3149=(
BOUNDED_CURVE()
B_SPLINE_CURVE(2,(#26475,#26476,#26477),.UNSPECIFIED.,.F.,.F.)
B_SPLINE_CURVE_WITH_KNOTS((3,3),(0.00176314208017924,0.0605078201286807),
 .UNSPECIFIED.)
CURVE()
GEOMETRIC_REPRESENTATION_ITEM()
RATIONAL_B_SPLINE_CURVE((1.00020515445013,1.00359200155151,1.00492385476097))
REPRESENTATION_ITEM('')
);
#3150=(
BOUNDED_CURVE()
B_SPLINE_CURVE(2,(#26479,#26480,#26481),.UNSPECIFIED.,.F.,.F.)
B_SPLINE_CURVE_WITH_KNOTS((3,3),(0.136653338911782,0.195398016960284),
 .UNSPECIFIED.)
CURVE()
GEOMETRIC_REPRESENTATION_ITEM()
RATIONAL_B_SPLINE_CURVE((1.00492385476095,1.00359200155149,1.00020515445012))
REPRESENTATION_ITEM('')
);
#3151=(
BOUNDED_CURVE()
B_SPLINE_CURVE(2,(#26493,#26494,#26495),.UNSPECIFIED.,.F.,.F.)
B_SPLINE_CURVE_WITH_KNOTS((3,3),(0.00176314208017894,0.06050782012868),
 .UNSPECIFIED.)
CURVE()
GEOMETRIC_REPRESENTATION_ITEM()
RATIONAL_B_SPLINE_CURVE((1.00020515445013,1.00359200155151,1.00492385476098))
REPRESENTATION_ITEM('')
);
#3152=(
BOUNDED_CURVE()
B_SPLINE_CURVE(2,(#26516,#26517,#26518),.UNSPECIFIED.,.F.,.F.)
B_SPLINE_CURVE_WITH_KNOTS((3,3),(0.00176314208017899,0.0605078201286809),
 .UNSPECIFIED.)
CURVE()
GEOMETRIC_REPRESENTATION_ITEM()
RATIONAL_B_SPLINE_CURVE((1.00020515445012,1.00359200155149,1.00492385476096))
REPRESENTATION_ITEM('')
);
#3153=(
BOUNDED_CURVE()
B_SPLINE_CURVE(2,(#26520,#26521,#26522),.UNSPECIFIED.,.F.,.F.)
B_SPLINE_CURVE_WITH_KNOTS((3,3),(0.136653338911781,0.195398016960282),
 .UNSPECIFIED.)
CURVE()
GEOMETRIC_REPRESENTATION_ITEM()
RATIONAL_B_SPLINE_CURVE((1.00492385476097,1.0035920015515,1.00020515445013))
REPRESENTATION_ITEM('')
);
#3154=(
BOUNDED_CURVE()
B_SPLINE_CURVE(2,(#26534,#26535,#26536),.UNSPECIFIED.,.F.,.F.)
B_SPLINE_CURVE_WITH_KNOTS((3,3),(0.00176314208017926,0.0605078201286816),
 .UNSPECIFIED.)
CURVE()
GEOMETRIC_REPRESENTATION_ITEM()
RATIONAL_B_SPLINE_CURVE((1.00020515445013,1.00359200155149,1.00492385476096))
REPRESENTATION_ITEM('')
);
#3155=(
BOUNDED_CURVE()
B_SPLINE_CURVE(2,(#26538,#26539,#26540),.UNSPECIFIED.,.F.,.F.)
B_SPLINE_CURVE_WITH_KNOTS((3,3),(0.136653338911783,0.195398016960284),
 .UNSPECIFIED.)
CURVE()
GEOMETRIC_REPRESENTATION_ITEM()
RATIONAL_B_SPLINE_CURVE((1.00492385476097,1.00359200155151,1.00020515445013))
REPRESENTATION_ITEM('')
);
#3156=(
BOUNDED_CURVE()
B_SPLINE_CURVE(2,(#26552,#26553,#26554),.UNSPECIFIED.,.F.,.F.)
B_SPLINE_CURVE_WITH_KNOTS((3,3),(0.00176314208017907,0.0605078201286811),
 .UNSPECIFIED.)
CURVE()
GEOMETRIC_REPRESENTATION_ITEM()
RATIONAL_B_SPLINE_CURVE((1.00020515445012,1.00359200155149,1.00492385476096))
REPRESENTATION_ITEM('')
);
#3157=(
BOUNDED_CURVE()
B_SPLINE_CURVE(2,(#26556,#26557,#26558),.UNSPECIFIED.,.F.,.F.)
B_SPLINE_CURVE_WITH_KNOTS((3,3),(0.136653338911777,0.19539801696028),
 .UNSPECIFIED.)
CURVE()
GEOMETRIC_REPRESENTATION_ITEM()
RATIONAL_B_SPLINE_CURVE((1.00492385476094,1.00359200155149,1.00020515445012))
REPRESENTATION_ITEM('')
);
#3158=(
BOUNDED_CURVE()
B_SPLINE_CURVE(2,(#26570,#26571,#26572),.UNSPECIFIED.,.F.,.F.)
B_SPLINE_CURVE_WITH_KNOTS((3,3),(0.00176314208017916,0.0605078201286813),
 .UNSPECIFIED.)
CURVE()
GEOMETRIC_REPRESENTATION_ITEM()
RATIONAL_B_SPLINE_CURVE((1.00020515445012,1.00359200155149,1.00492385476095))
REPRESENTATION_ITEM('')
);
#3159=(
BOUNDED_CURVE()
B_SPLINE_CURVE(2,(#26574,#26575,#26576),.UNSPECIFIED.,.F.,.F.)
B_SPLINE_CURVE_WITH_KNOTS((3,3),(0.136653338911781,0.195398016960283),
 .UNSPECIFIED.)
CURVE()
GEOMETRIC_REPRESENTATION_ITEM()
RATIONAL_B_SPLINE_CURVE((1.00492385476096,1.0035920015515,1.00020515445013))
REPRESENTATION_ITEM('')
);
#3160=(
BOUNDED_CURVE()
B_SPLINE_CURVE(2,(#26588,#26589,#26590),.UNSPECIFIED.,.F.,.F.)
B_SPLINE_CURVE_WITH_KNOTS((3,3),(0.00176314208017902,0.060507820128681),
 .UNSPECIFIED.)
CURVE()
GEOMETRIC_REPRESENTATION_ITEM()
RATIONAL_B_SPLINE_CURVE((1.00020515445012,1.00359200155149,1.00492385476096))
REPRESENTATION_ITEM('')
);
#3161=(
BOUNDED_CURVE()
B_SPLINE_CURVE(2,(#26592,#26593,#26594),.UNSPECIFIED.,.F.,.F.)
B_SPLINE_CURVE_WITH_KNOTS((3,3),(0.13665333891178,0.195398016960282),
 .UNSPECIFIED.)
CURVE()
GEOMETRIC_REPRESENTATION_ITEM()
RATIONAL_B_SPLINE_CURVE((1.00492385476095,1.00359200155149,1.00020515445012))
REPRESENTATION_ITEM('')
);
#3162=(
BOUNDED_CURVE()
B_SPLINE_CURVE(2,(#26606,#26607,#26608),.UNSPECIFIED.,.F.,.F.)
B_SPLINE_CURVE_WITH_KNOTS((3,3),(0.00176314208017895,0.0605078201286814),
 .UNSPECIFIED.)
CURVE()
GEOMETRIC_REPRESENTATION_ITEM()
RATIONAL_B_SPLINE_CURVE((1.00020515445012,1.00359200155149,1.00492385476095))
REPRESENTATION_ITEM('')
);
#3163=(
BOUNDED_CURVE()
B_SPLINE_CURVE(2,(#26610,#26611,#26612),.UNSPECIFIED.,.F.,.F.)
B_SPLINE_CURVE_WITH_KNOTS((3,3),(0.136653338911781,0.195398016960283),
 .UNSPECIFIED.)
CURVE()
GEOMETRIC_REPRESENTATION_ITEM()
RATIONAL_B_SPLINE_CURVE((1.00492385476096,1.00359200155149,1.00020515445012))
REPRESENTATION_ITEM('')
);
#3164=(
BOUNDED_CURVE()
B_SPLINE_CURVE(2,(#26624,#26625,#26626),.UNSPECIFIED.,.F.,.F.)
B_SPLINE_CURVE_WITH_KNOTS((3,3),(0.00176314208017911,0.0605078201286809),
 .UNSPECIFIED.)
CURVE()
GEOMETRIC_REPRESENTATION_ITEM()
RATIONAL_B_SPLINE_CURVE((1.00020515445013,1.0035920015515,1.00492385476096))
REPRESENTATION_ITEM('')
);
#3165=(
BOUNDED_CURVE()
B_SPLINE_CURVE(2,(#26628,#26629,#26630),.UNSPECIFIED.,.F.,.F.)
B_SPLINE_CURVE_WITH_KNOTS((3,3),(0.136653338911778,0.19539801696028),
 .UNSPECIFIED.)
CURVE()
GEOMETRIC_REPRESENTATION_ITEM()
RATIONAL_B_SPLINE_CURVE((1.00492385476096,1.0035920015515,1.00020515445013))
REPRESENTATION_ITEM('')
);
#3166=(
BOUNDED_CURVE()
B_SPLINE_CURVE(2,(#26642,#26643,#26644),.UNSPECIFIED.,.F.,.F.)
B_SPLINE_CURVE_WITH_KNOTS((3,3),(0.00176314208017945,0.0605078201286828),
 .UNSPECIFIED.)
CURVE()
GEOMETRIC_REPRESENTATION_ITEM()
RATIONAL_B_SPLINE_CURVE((1.00020515445012,1.00359200155148,1.00492385476094))
REPRESENTATION_ITEM('')
);
#3167=(
BOUNDED_CURVE()
B_SPLINE_CURVE(2,(#26646,#26647,#26648),.UNSPECIFIED.,.F.,.F.)
B_SPLINE_CURVE_WITH_KNOTS((3,3),(0.136653338911782,0.195398016960283),
 .UNSPECIFIED.)
CURVE()
GEOMETRIC_REPRESENTATION_ITEM()
RATIONAL_B_SPLINE_CURVE((1.00492385476098,1.00359200155151,1.00020515445013))
REPRESENTATION_ITEM('')
);
#3168=(
BOUNDED_CURVE()
B_SPLINE_CURVE(2,(#30191,#30192,#30193),.UNSPECIFIED.,.F.,.F.)
B_SPLINE_CURVE_WITH_KNOTS((3,3),(0.0476157841635492,0.475541178108418),
 .UNSPECIFIED.)
CURVE()
GEOMETRIC_REPRESENTATION_ITEM()
RATIONAL_B_SPLINE_CURVE((1.03978013844038,1.20063468565316,1.03978013844038))
REPRESENTATION_ITEM('')
);
#3169=(
BOUNDED_CURVE()
B_SPLINE_CURVE(2,(#30195,#30196,#30197),.UNSPECIFIED.,.F.,.F.)
B_SPLINE_CURVE_WITH_KNOTS((3,3),(0.0476157841635493,0.475541178108419),
 .UNSPECIFIED.)
CURVE()
GEOMETRIC_REPRESENTATION_ITEM()
RATIONAL_B_SPLINE_CURVE((1.03978013844038,1.20063468565316,1.03978013844038))
REPRESENTATION_ITEM('')
);
#3170=(
BOUNDED_CURVE()
B_SPLINE_CURVE(2,(#30199,#30200,#30201),.UNSPECIFIED.,.F.,.F.)
B_SPLINE_CURVE_WITH_KNOTS((3,3),(0.0476157841635493,0.475541178108419),
 .UNSPECIFIED.)
CURVE()
GEOMETRIC_REPRESENTATION_ITEM()
RATIONAL_B_SPLINE_CURVE((1.03978013844038,1.20063468565316,1.03978013844038))
REPRESENTATION_ITEM('')
);
#3171=(
BOUNDED_CURVE()
B_SPLINE_CURVE(2,(#30203,#30204,#30205),.UNSPECIFIED.,.F.,.F.)
B_SPLINE_CURVE_WITH_KNOTS((3,3),(0.0476157841635494,0.475541178108419),
 .UNSPECIFIED.)
CURVE()
GEOMETRIC_REPRESENTATION_ITEM()
RATIONAL_B_SPLINE_CURVE((1.03978013844038,1.20063468565316,1.03978013844038))
REPRESENTATION_ITEM('')
);
#3172=(
BOUNDED_CURVE()
B_SPLINE_CURVE(2,(#30207,#30208,#30209),.UNSPECIFIED.,.F.,.F.)
B_SPLINE_CURVE_WITH_KNOTS((3,3),(0.261578481135984,0.475541178108418),
 .UNSPECIFIED.)
CURVE()
GEOMETRIC_REPRESENTATION_ITEM()
RATIONAL_B_SPLINE_CURVE((1.12020741204677,1.12020741204677,1.03978013844038))
REPRESENTATION_ITEM('')
);
#3173=(
BOUNDED_CURVE()
B_SPLINE_CURVE(2,(#30214,#30215,#30216),.UNSPECIFIED.,.F.,.F.)
B_SPLINE_CURVE_WITH_KNOTS((3,3),(0.0476157841635493,0.261578481135984),
 .UNSPECIFIED.)
CURVE()
GEOMETRIC_REPRESENTATION_ITEM()
RATIONAL_B_SPLINE_CURVE((1.03978013844038,1.12020741204677,1.12020741204677))
REPRESENTATION_ITEM('')
);
#3174=(
BOUNDED_CURVE()
B_SPLINE_CURVE(2,(#30217,#30218,#30219),.UNSPECIFIED.,.F.,.F.)
B_SPLINE_CURVE_WITH_KNOTS((3,3),(0.0476157841635491,0.475541178108418),
 .UNSPECIFIED.)
CURVE()
GEOMETRIC_REPRESENTATION_ITEM()
RATIONAL_B_SPLINE_CURVE((1.03978013844038,1.20063468565316,1.03978013844038))
REPRESENTATION_ITEM('')
);
#3175=(
BOUNDED_CURVE()
B_SPLINE_CURVE(2,(#34276,#34277,#34278),.UNSPECIFIED.,.F.,.F.)
B_SPLINE_CURVE_WITH_KNOTS((3,3),(-1.30181351501822,-0.516279708895519),
 .UNSPECIFIED.)
CURVE()
GEOMETRIC_REPRESENTATION_ITEM()
RATIONAL_B_SPLINE_CURVE((0.98985802419273,0.918917809350684,1.))
REPRESENTATION_ITEM('')
);
#3176=(
BOUNDED_CURVE()
B_SPLINE_CURVE(2,(#34308,#34309,#34310),.UNSPECIFIED.,.F.,.F.)
B_SPLINE_CURVE_WITH_KNOTS((3,3),(0.0719702485074244,0.107109429758004),
 .UNSPECIFIED.)
CURVE()
GEOMETRIC_REPRESENTATION_ITEM()
RATIONAL_B_SPLINE_CURVE((1.0121972483025,1.01317411304727,1.0121972483025))
REPRESENTATION_ITEM('')
);
#3177=(
BOUNDED_CURVE()
B_SPLINE_CURVE(2,(#34314,#34315,#34316),.UNSPECIFIED.,.F.,.F.)
B_SPLINE_CURVE_WITH_KNOTS((3,3),(0.0719702485074238,0.107109429758003),
 .UNSPECIFIED.)
CURVE()
GEOMETRIC_REPRESENTATION_ITEM()
RATIONAL_B_SPLINE_CURVE((1.0121972483025,1.01317411304726,1.0121972483025))
REPRESENTATION_ITEM('')
);
#3178=(
BOUNDED_CURVE()
B_SPLINE_CURVE(2,(#34320,#34321,#34322),.UNSPECIFIED.,.F.,.F.)
B_SPLINE_CURVE_WITH_KNOTS((3,3),(0.0663017168058462,0.456855245466122),
 .UNSPECIFIED.)
CURVE()
GEOMETRIC_REPRESENTATION_ITEM()
RATIONAL_B_SPLINE_CURVE((1.05321457643448,1.18720024765905,1.05321457643448))
REPRESENTATION_ITEM('')
);
#3179=(
BOUNDED_CURVE()
B_SPLINE_CURVE(2,(#34325,#34326,#34327),.UNSPECIFIED.,.F.,.F.)
B_SPLINE_CURVE_WITH_KNOTS((3,3),(0.0663017168058461,0.456855245466121),
 .UNSPECIFIED.)
CURVE()
GEOMETRIC_REPRESENTATION_ITEM()
RATIONAL_B_SPLINE_CURVE((1.05321457643448,1.18720024765905,1.05321457643448))
REPRESENTATION_ITEM('')
);
#3180=(
BOUNDED_CURVE()
B_SPLINE_CURVE(2,(#34330,#34331,#34332),.UNSPECIFIED.,.F.,.F.)
B_SPLINE_CURVE_WITH_KNOTS((3,3),(0.0663017168058462,0.456855245466121),
 .UNSPECIFIED.)
CURVE()
GEOMETRIC_REPRESENTATION_ITEM()
RATIONAL_B_SPLINE_CURVE((1.05321457643448,1.18720024765905,1.05321457643448))
REPRESENTATION_ITEM('')
);
#3181=(
BOUNDED_CURVE()
B_SPLINE_CURVE(2,(#34334,#34335,#34336),.UNSPECIFIED.,.F.,.F.)
B_SPLINE_CURVE_WITH_KNOTS((3,3),(0.0719702485074243,0.107109429758004),
 .UNSPECIFIED.)
CURVE()
GEOMETRIC_REPRESENTATION_ITEM()
RATIONAL_B_SPLINE_CURVE((1.0121972483025,1.01317411304726,1.0121972483025))
REPRESENTATION_ITEM('')
);
#3182=(
BOUNDED_CURVE()
B_SPLINE_CURVE(2,(#34338,#34339,#34340),.UNSPECIFIED.,.F.,.F.)
B_SPLINE_CURVE_WITH_KNOTS((3,3),(0.0663017168058464,0.456855245466122),
 .UNSPECIFIED.)
CURVE()
GEOMETRIC_REPRESENTATION_ITEM()
RATIONAL_B_SPLINE_CURVE((1.05321457643448,1.18720024765905,1.05321457643448))
REPRESENTATION_ITEM('')
);
#3183=(
BOUNDED_CURVE()
B_SPLINE_CURVE(2,(#34342,#34343,#34344),.UNSPECIFIED.,.F.,.F.)
B_SPLINE_CURVE_WITH_KNOTS((3,3),(0.0719702485074242,0.107109429758004),
 .UNSPECIFIED.)
CURVE()
GEOMETRIC_REPRESENTATION_ITEM()
RATIONAL_B_SPLINE_CURVE((1.0121972483025,1.01317411304726,1.0121972483025))
REPRESENTATION_ITEM('')
);
#3184=(
BOUNDED_CURVE()
B_SPLINE_CURVE(2,(#34346,#34347,#34348),.UNSPECIFIED.,.F.,.F.)
B_SPLINE_CURVE_WITH_KNOTS((3,3),(0.261578481135983,0.456855245466121),
 .UNSPECIFIED.)
CURVE()
GEOMETRIC_REPRESENTATION_ITEM()
RATIONAL_B_SPLINE_CURVE((1.12020741204677,1.12020741204677,1.05321457643449))
REPRESENTATION_ITEM('')
);
#3185=(
BOUNDED_CURVE()
B_SPLINE_CURVE(2,(#34353,#34354,#34355),.UNSPECIFIED.,.F.,.F.)
B_SPLINE_CURVE_WITH_KNOTS((3,3),(0.0663017168058461,0.261578481135983),
 .UNSPECIFIED.)
CURVE()
GEOMETRIC_REPRESENTATION_ITEM()
RATIONAL_B_SPLINE_CURVE((1.05321457643448,1.12020741204677,1.12020741204677))
REPRESENTATION_ITEM('')
);
#3186=(
BOUNDED_CURVE()
B_SPLINE_CURVE(2,(#34357,#34358,#34359),.UNSPECIFIED.,.F.,.F.)
B_SPLINE_CURVE_WITH_KNOTS((3,3),(0.0719702485074242,0.107109429758004),
 .UNSPECIFIED.)
CURVE()
GEOMETRIC_REPRESENTATION_ITEM()
RATIONAL_B_SPLINE_CURVE((1.0121972483025,1.01317411304727,1.0121972483025))
REPRESENTATION_ITEM('')
);
#3187=(
BOUNDED_CURVE()
B_SPLINE_CURVE(2,(#34361,#34362,#34363),.UNSPECIFIED.,.F.,.F.)
B_SPLINE_CURVE_WITH_KNOTS((3,3),(0.066301716805846,0.456855245466121),
 .UNSPECIFIED.)
CURVE()
GEOMETRIC_REPRESENTATION_ITEM()
RATIONAL_B_SPLINE_CURVE((1.05321457643448,1.18720024765905,1.05321457643448))
REPRESENTATION_ITEM('')
);
#3188=(
BOUNDED_CURVE()
B_SPLINE_CURVE(2,(#34365,#34366,#34367),.UNSPECIFIED.,.F.,.F.)
B_SPLINE_CURVE_WITH_KNOTS((3,3),(0.0719702485074249,0.107109429758004),
 .UNSPECIFIED.)
CURVE()
GEOMETRIC_REPRESENTATION_ITEM()
RATIONAL_B_SPLINE_CURVE((1.0121972483025,1.01317411304726,1.0121972483025))
REPRESENTATION_ITEM('')
);
#3189=(
BOUNDED_CURVE()
B_SPLINE_CURVE(2,(#34369,#34370,#34371),.UNSPECIFIED.,.F.,.F.)
B_SPLINE_CURVE_WITH_KNOTS((3,3),(0.0663017168058463,0.456855245466121),
 .UNSPECIFIED.)
CURVE()
GEOMETRIC_REPRESENTATION_ITEM()
RATIONAL_B_SPLINE_CURVE((1.05321457643448,1.18720024765905,1.05321457643448))
REPRESENTATION_ITEM('')
);
#3190=(
BOUNDED_CURVE()
B_SPLINE_CURVE(2,(#34372,#34373,#34374),.UNSPECIFIED.,.F.,.F.)
B_SPLINE_CURVE_WITH_KNOTS((3,3),(0.0719702485074235,0.107109429758003),
 .UNSPECIFIED.)
CURVE()
GEOMETRIC_REPRESENTATION_ITEM()
RATIONAL_B_SPLINE_CURVE((1.0121972483025,1.01317411304727,1.0121972483025))
REPRESENTATION_ITEM('')
);
#3191=(
BOUNDED_CURVE()
B_SPLINE_CURVE(2,(#34397,#34398,#34399),.UNSPECIFIED.,.F.,.F.)
B_SPLINE_CURVE_WITH_KNOTS((3,3),(0.0719702485074245,0.107109429758004),
 .UNSPECIFIED.)
CURVE()
GEOMETRIC_REPRESENTATION_ITEM()
RATIONAL_B_SPLINE_CURVE((1.0121972483025,1.01317411304727,1.0121972483025))
REPRESENTATION_ITEM('')
);
#3192=(
BOUNDED_CURVE()
B_SPLINE_CURVE(2,(#34403,#34404,#34405),.UNSPECIFIED.,.F.,.F.)
B_SPLINE_CURVE_WITH_KNOTS((3,3),(0.0663017168058461,0.456855245466121),
 .UNSPECIFIED.)
CURVE()
GEOMETRIC_REPRESENTATION_ITEM()
RATIONAL_B_SPLINE_CURVE((1.05321457643448,1.18720024765905,1.05321457643448))
REPRESENTATION_ITEM('')
);
#3193=(
BOUNDED_CURVE()
B_SPLINE_CURVE(2,(#34411,#34412,#34413),.UNSPECIFIED.,.F.,.F.)
B_SPLINE_CURVE_WITH_KNOTS((3,3),(0.0663017168058461,0.261578481135983),
 .UNSPECIFIED.)
CURVE()
GEOMETRIC_REPRESENTATION_ITEM()
RATIONAL_B_SPLINE_CURVE((1.05321457643448,1.12020741204677,1.12020741204677))
REPRESENTATION_ITEM('')
);
#3194=(
BOUNDED_CURVE()
B_SPLINE_CURVE(2,(#34414,#34415,#34416),.UNSPECIFIED.,.F.,.F.)
B_SPLINE_CURVE_WITH_KNOTS((3,3),(0.0719702485074254,0.107109429758005),
 .UNSPECIFIED.)
CURVE()
GEOMETRIC_REPRESENTATION_ITEM()
RATIONAL_B_SPLINE_CURVE((1.0121972483025,1.01317411304726,1.0121972483025))
REPRESENTATION_ITEM('')
);
#3195=(
BOUNDED_CURVE()
B_SPLINE_CURVE(2,(#34417,#34418,#34419),.UNSPECIFIED.,.F.,.F.)
B_SPLINE_CURVE_WITH_KNOTS((3,3),(0.0663017168058463,0.456855245466121),
 .UNSPECIFIED.)
CURVE()
GEOMETRIC_REPRESENTATION_ITEM()
RATIONAL_B_SPLINE_CURVE((1.05321457643448,1.18720024765905,1.05321457643448))
REPRESENTATION_ITEM('')
);
#3196=(
BOUNDED_CURVE()
B_SPLINE_CURVE(2,(#34421,#34422,#34423),.UNSPECIFIED.,.F.,.F.)
B_SPLINE_CURVE_WITH_KNOTS((3,3),(0.0719702485074251,0.107109429758005),
 .UNSPECIFIED.)
CURVE()
GEOMETRIC_REPRESENTATION_ITEM()
RATIONAL_B_SPLINE_CURVE((1.0121972483025,1.01317411304726,1.01219724830249))
REPRESENTATION_ITEM('')
);
#3197=(
BOUNDED_CURVE()
B_SPLINE_CURVE(2,(#34425,#34426,#34427),.UNSPECIFIED.,.F.,.F.)
B_SPLINE_CURVE_WITH_KNOTS((3,3),(0.0663017168058462,0.456855245466121),
 .UNSPECIFIED.)
CURVE()
GEOMETRIC_REPRESENTATION_ITEM()
RATIONAL_B_SPLINE_CURVE((1.05321457643448,1.18720024765905,1.05321457643448))
REPRESENTATION_ITEM('')
);
#3198=(
BOUNDED_CURVE()
B_SPLINE_CURVE(2,(#34429,#34430,#34431),.UNSPECIFIED.,.F.,.F.)
B_SPLINE_CURVE_WITH_KNOTS((3,3),(0.0719702485074238,0.107109429758004),
 .UNSPECIFIED.)
CURVE()
GEOMETRIC_REPRESENTATION_ITEM()
RATIONAL_B_SPLINE_CURVE((1.0121972483025,1.01317411304727,1.0121972483025))
REPRESENTATION_ITEM('')
);
#3199=(
BOUNDED_CURVE()
B_SPLINE_CURVE(2,(#34433,#34434,#34435),.UNSPECIFIED.,.F.,.F.)
B_SPLINE_CURVE_WITH_KNOTS((3,3),(0.0663017168058462,0.456855245466121),
 .UNSPECIFIED.)
CURVE()
GEOMETRIC_REPRESENTATION_ITEM()
RATIONAL_B_SPLINE_CURVE((1.05321457643448,1.18720024765905,1.05321457643448))
REPRESENTATION_ITEM('')
);
#3200=(
BOUNDED_CURVE()
B_SPLINE_CURVE(2,(#34437,#34438,#34439),.UNSPECIFIED.,.F.,.F.)
B_SPLINE_CURVE_WITH_KNOTS((3,3),(0.0719702485074251,0.107109429758005),
 .UNSPECIFIED.)
CURVE()
GEOMETRIC_REPRESENTATION_ITEM()
RATIONAL_B_SPLINE_CURVE((1.0121972483025,1.01317411304726,1.0121972483025))
REPRESENTATION_ITEM('')
);
#3201=(
BOUNDED_CURVE()
B_SPLINE_CURVE(2,(#34440,#34441,#34442),.UNSPECIFIED.,.F.,.F.)
B_SPLINE_CURVE_WITH_KNOTS((3,3),(0.261578481135983,0.456855245466121),
 .UNSPECIFIED.)
CURVE()
GEOMETRIC_REPRESENTATION_ITEM()
RATIONAL_B_SPLINE_CURVE((1.12020741204677,1.12020741204677,1.05321457643448))
REPRESENTATION_ITEM('')
);
#3202=(
BOUNDED_CURVE()
B_SPLINE_CURVE(2,(#37126,#37127,#37128),.UNSPECIFIED.,.F.,.F.)
B_SPLINE_CURVE_WITH_KNOTS((3,3),(-1.33896509897879,-0.513408172091738),
 .UNSPECIFIED.)
CURVE()
GEOMETRIC_REPRESENTATION_ITEM()
RATIONAL_B_SPLINE_CURVE((0.98929230069637,0.910813429578529,1.))
REPRESENTATION_ITEM('')
);
#3203=LINE('',#19753,#4442);
#3204=LINE('',#19755,#4443);
#3205=LINE('',#19757,#4444);
#3206=LINE('',#19763,#4445);
#3207=LINE('',#19773,#4446);
#3208=LINE('',#19775,#4447);
#3209=LINE('',#19776,#4448);
#3210=LINE('',#19792,#4449);
#3211=LINE('',#19795,#4450);
#3212=LINE('',#19796,#4451);
#3213=LINE('',#19800,#4452);
#3214=LINE('',#19802,#4453);
#3215=LINE('',#19803,#4454);
#3216=LINE('',#19807,#4455);
#3217=LINE('',#19808,#4456);
#3218=LINE('',#19809,#4457);
#3219=LINE('',#19814,#4458);
#3220=LINE('',#19822,#4459);
#3221=LINE('',#19823,#4460);
#3222=LINE('',#19825,#4461);
#3223=LINE('',#19827,#4462);
#3224=LINE('',#19832,#4463);
#3225=LINE('',#19833,#4464);
#3226=LINE('',#19841,#4465);
#3227=LINE('',#19843,#4466);
#3228=LINE('',#19844,#4467);
#3229=LINE('',#19849,#4468);
#3230=LINE('',#19852,#4469);
#3231=LINE('',#19853,#4470);
#3232=LINE('',#19858,#4471);
#3233=LINE('',#19862,#4472);
#3234=LINE('',#19864,#4473);
#3235=LINE('',#19867,#4474);
#3236=LINE('',#19869,#4475);
#3237=LINE('',#19876,#4476);
#3238=LINE('',#19885,#4477);
#3239=LINE('',#19887,#4478);
#3240=LINE('',#19888,#4479);
#3241=LINE('',#19894,#4480);
#3242=LINE('',#19896,#4481);
#3243=LINE('',#19897,#4482);
#3244=LINE('',#19900,#4483);
#3245=LINE('',#19901,#4484);
#3246=LINE('',#19905,#4485);
#3247=LINE('',#19906,#4486);
#3248=LINE('',#19907,#4487);
#3249=LINE('',#19912,#4488);
#3250=LINE('',#19919,#4489);
#3251=LINE('',#19920,#4490);
#3252=LINE('',#19924,#4491);
#3253=LINE('',#19926,#4492);
#3254=LINE('',#19928,#4493);
#3255=LINE('',#19929,#4494);
#3256=LINE('',#19933,#4495);
#3257=LINE('',#19934,#4496);
#3258=LINE('',#19935,#4497);
#3259=LINE('',#19940,#4498);
#3260=LINE('',#19948,#4499);
#3261=LINE('',#19949,#4500);
#3262=LINE('',#19968,#4501);
#3263=LINE('',#19971,#4502);
#3264=LINE('',#19976,#4503);
#3265=LINE('',#19979,#4504);
#3266=LINE('',#19980,#4505);
#3267=LINE('',#19988,#4506);
#3268=LINE('',#19990,#4507);
#3269=LINE('',#19992,#4508);
#3270=LINE('',#19993,#4509);
#3271=LINE('',#19998,#4510);
#3272=LINE('',#20003,#4511);
#3273=LINE('',#20004,#4512);
#3274=LINE('',#20005,#4513);
#3275=LINE('',#20010,#4514);
#3276=LINE('',#20014,#4515);
#3277=LINE('',#20016,#4516);
#3278=LINE('',#20017,#4517);
#3279=LINE('',#20020,#4518);
#3280=LINE('',#20025,#4519);
#3281=LINE('',#20027,#4520);
#3282=LINE('',#20036,#4521);
#3283=LINE('',#20041,#4522);
#3284=LINE('',#20045,#4523);
#3285=LINE('',#20047,#4524);
#3286=LINE('',#20049,#4525);
#3287=LINE('',#20050,#4526);
#3288=LINE('',#20054,#4527);
#3289=LINE('',#20056,#4528);
#3290=LINE('',#20058,#4529);
#3291=LINE('',#20059,#4530);
#3292=LINE('',#20062,#4531);
#3293=LINE('',#20064,#4532);
#3294=LINE('',#20065,#4533);
#3295=LINE('',#20069,#4534);
#3296=LINE('',#20075,#4535);
#3297=LINE('',#20076,#4536);
#3298=LINE('',#20078,#4537);
#3299=LINE('',#20079,#4538);
#3300=LINE('',#20083,#4539);
#3301=LINE('',#20089,#4540);
#3302=LINE('',#20090,#4541);
#3303=LINE('',#20091,#4542);
#3304=LINE('',#20095,#4543);
#3305=LINE('',#20099,#4544);
#3306=LINE('',#20100,#4545);
#3307=LINE('',#20105,#4546);
#3308=LINE('',#20110,#4547);
#3309=LINE('',#20111,#4548);
#3310=LINE('',#20113,#4549);
#3311=LINE('',#20114,#4550);
#3312=LINE('',#20117,#4551);
#3313=LINE('',#20121,#4552);
#3314=LINE('',#20123,#4553);
#3315=LINE('',#20125,#4554);
#3316=LINE('',#20127,#4555);
#3317=LINE('',#20129,#4556);
#3318=LINE('',#20133,#4557);
#3319=LINE('',#20135,#4558);
#3320=LINE('',#20138,#4559);
#3321=LINE('',#20139,#4560);
#3322=LINE('',#20141,#4561);
#3323=LINE('',#20143,#4562);
#3324=LINE('',#20145,#4563);
#3325=LINE('',#20148,#4564);
#3326=LINE('',#20152,#4565);
#3327=LINE('',#20154,#4566);
#3328=LINE('',#20158,#4567);
#3329=LINE('',#20160,#4568);
#3330=LINE('',#20162,#4569);
#3331=LINE('',#20164,#4570);
#3332=LINE('',#20166,#4571);
#3333=LINE('',#20170,#4572);
#3334=LINE('',#20172,#4573);
#3335=LINE('',#20174,#4574);
#3336=LINE('',#20180,#4575);
#3337=LINE('',#20182,#4576);
#3338=LINE('',#20188,#4577);
#3339=LINE('',#20190,#4578);
#3340=LINE('',#20196,#4579);
#3341=LINE('',#20202,#4580);
#3342=LINE('',#20204,#4581);
#3343=LINE('',#20205,#4582);
#3344=LINE('',#20209,#4583);
#3345=LINE('',#20210,#4584);
#3346=LINE('',#20212,#4585);
#3347=LINE('',#20213,#4586);
#3348=LINE('',#20216,#4587);
#3349=LINE('',#20217,#4588);
#3350=LINE('',#20221,#4589);
#3351=LINE('',#20224,#4590);
#3352=LINE('',#20225,#4591);
#3353=LINE('',#20229,#4592);
#3354=LINE('',#20230,#4593);
#3355=LINE('',#20236,#4594);
#3356=LINE('',#20239,#4595);
#3357=LINE('',#20241,#4596);
#3358=LINE('',#20243,#4597);
#3359=LINE('',#20244,#4598);
#3360=LINE('',#20247,#4599);
#3361=LINE('',#20249,#4600);
#3362=LINE('',#20254,#4601);
#3363=LINE('',#20263,#4602);
#3364=LINE('',#20268,#4603);
#3365=LINE('',#20271,#4604);
#3366=LINE('',#20272,#4605);
#3367=LINE('',#20275,#4606);
#3368=LINE('',#20276,#4607);
#3369=LINE('',#20280,#4608);
#3370=LINE('',#20285,#4609);
#3371=LINE('',#20287,#4610);
#3372=LINE('',#20288,#4611);
#3373=LINE('',#20291,#4612);
#3374=LINE('',#20295,#4613);
#3375=LINE('',#20297,#4614);
#3376=LINE('',#20305,#4615);
#3377=LINE('',#20306,#4616);
#3378=LINE('',#20307,#4617);
#3379=LINE('',#20315,#4618);
#3380=LINE('',#20321,#4619);
#3381=LINE('',#20322,#4620);
#3382=LINE('',#20323,#4621);
#3383=LINE('',#20326,#4622);
#3384=LINE('',#20330,#4623);
#3385=LINE('',#20344,#4624);
#3386=LINE('',#20346,#4625);
#3387=LINE('',#20347,#4626);
#3388=LINE('',#20349,#4627);
#3389=LINE('',#20350,#4628);
#3390=LINE('',#20358,#4629);
#3391=LINE('',#20366,#4630);
#3392=LINE('',#20369,#4631);
#3393=LINE('',#20373,#4632);
#3394=LINE('',#20376,#4633);
#3395=LINE('',#20384,#4634);
#3396=LINE('',#20396,#4635);
#3397=LINE('',#20423,#4636);
#3398=LINE('',#20425,#4637);
#3399=LINE('',#20429,#4638);
#3400=LINE('',#20430,#4639);
#3401=LINE('',#20433,#4640);
#3402=LINE('',#20434,#4641);
#3403=LINE('',#20438,#4642);
#3404=LINE('',#20445,#4643);
#3405=LINE('',#20453,#4644);
#3406=LINE('',#20460,#4645);
#3407=LINE('',#20486,#4646);
#3408=LINE('',#20487,#4647);
#3409=LINE('',#20488,#4648);
#3410=LINE('',#20499,#4649);
#3411=LINE('',#20502,#4650);
#3412=LINE('',#20505,#4651);
#3413=LINE('',#20510,#4652);
#3414=LINE('',#20512,#4653);
#3415=LINE('',#20514,#4654);
#3416=LINE('',#20516,#4655);
#3417=LINE('',#20518,#4656);
#3418=LINE('',#20520,#4657);
#3419=LINE('',#20527,#4658);
#3420=LINE('',#20529,#4659);
#3421=LINE('',#20531,#4660);
#3422=LINE('',#20532,#4661);
#3423=LINE('',#20536,#4662);
#3424=LINE('',#20542,#4663);
#3425=LINE('',#20543,#4664);
#3426=LINE('',#20544,#4665);
#3427=LINE('',#20547,#4666);
#3428=LINE('',#20549,#4667);
#3429=LINE('',#20550,#4668);
#3430=LINE('',#20553,#4669);
#3431=LINE('',#20557,#4670);
#3432=LINE('',#20558,#4671);
#3433=LINE('',#20561,#4672);
#3434=LINE('',#20563,#4673);
#3435=LINE('',#20564,#4674);
#3436=LINE('',#20567,#4675);
#3437=LINE('',#20571,#4676);
#3438=LINE('',#20572,#4677);
#3439=LINE('',#20574,#4678);
#3440=LINE('',#20577,#4679);
#3441=LINE('',#20579,#4680);
#3442=LINE('',#20581,#4681);
#3443=LINE('',#20583,#4682);
#3444=LINE('',#20585,#4683);
#3445=LINE('',#20586,#4684);
#3446=LINE('',#20590,#4685);
#3447=LINE('',#20592,#4686);
#3448=LINE('',#20594,#4687);
#3449=LINE('',#20595,#4688);
#3450=LINE('',#20599,#4689);
#3451=LINE('',#20605,#4690);
#3452=LINE('',#20606,#4691);
#3453=LINE('',#20607,#4692);
#3454=LINE('',#20610,#4693);
#3455=LINE('',#20612,#4694);
#3456=LINE('',#20613,#4695);
#3457=LINE('',#20616,#4696);
#3458=LINE('',#20620,#4697);
#3459=LINE('',#20621,#4698);
#3460=LINE('',#20625,#4699);
#3461=LINE('',#20627,#4700);
#3462=LINE('',#20628,#4701);
#3463=LINE('',#20632,#4702);
#3464=LINE('',#20633,#4703);
#3465=LINE('',#20634,#4704);
#3466=LINE('',#20638,#4705);
#3467=LINE('',#20639,#4706);
#3468=LINE('',#20641,#4707);
#3469=LINE('',#20642,#4708);
#3470=LINE('',#20646,#4709);
#3471=LINE('',#20647,#4710);
#3472=LINE('',#20649,#4711);
#3473=LINE('',#20650,#4712);
#3474=LINE('',#20653,#4713);
#3475=LINE('',#20654,#4714);
#3476=LINE('',#20657,#4715);
#3477=LINE('',#20658,#4716);
#3478=LINE('',#20661,#4717);
#3479=LINE('',#20663,#4718);
#3480=LINE('',#20664,#4719);
#3481=LINE('',#20669,#4720);
#3482=LINE('',#20673,#4721);
#3483=LINE('',#20676,#4722);
#3484=LINE('',#20681,#4723);
#3485=LINE('',#20685,#4724);
#3486=LINE('',#20688,#4725);
#3487=LINE('',#20691,#4726);
#3488=LINE('',#20696,#4727);
#3489=LINE('',#20698,#4728);
#3490=LINE('',#20700,#4729);
#3491=LINE('',#20702,#4730);
#3492=LINE('',#20704,#4731);
#3493=LINE('',#20705,#4732);
#3494=LINE('',#20708,#4733);
#3495=LINE('',#20710,#4734);
#3496=LINE('',#20711,#4735);
#3497=LINE('',#20714,#4736);
#3498=LINE('',#20715,#4737);
#3499=LINE('',#20718,#4738);
#3500=LINE('',#20720,#4739);
#3501=LINE('',#20721,#4740);
#3502=LINE('',#20724,#4741);
#3503=LINE('',#20725,#4742);
#3504=LINE('',#20727,#4743);
#3505=LINE('',#20729,#4744);
#3506=LINE('',#20731,#4745);
#3507=LINE('',#20732,#4746);
#3508=LINE('',#20734,#4747);
#3509=LINE('',#20736,#4748);
#3510=LINE('',#20739,#4749);
#3511=LINE('',#20744,#4750);
#3512=LINE('',#20746,#4751);
#3513=LINE('',#20748,#4752);
#3514=LINE('',#20750,#4753);
#3515=LINE('',#20752,#4754);
#3516=LINE('',#20753,#4755);
#3517=LINE('',#20756,#4756);
#3518=LINE('',#20758,#4757);
#3519=LINE('',#20759,#4758);
#3520=LINE('',#20762,#4759);
#3521=LINE('',#20766,#4760);
#3522=LINE('',#20767,#4761);
#3523=LINE('',#20771,#4762);
#3524=LINE('',#20773,#4763);
#3525=LINE('',#20775,#4764);
#3526=LINE('',#20776,#4765);
#3527=LINE('',#20779,#4766);
#3528=LINE('',#20781,#4767);
#3529=LINE('',#20782,#4768);
#3530=LINE('',#20786,#4769);
#3531=LINE('',#20788,#4770);
#3532=LINE('',#20790,#4771);
#3533=LINE('',#20791,#4772);
#3534=LINE('',#20794,#4773);
#3535=LINE('',#20796,#4774);
#3536=LINE('',#20797,#4775);
#3537=LINE('',#20799,#4776);
#3538=LINE('',#20800,#4777);
#3539=LINE('',#20802,#4778);
#3540=LINE('',#20803,#4779);
#3541=LINE('',#20805,#4780);
#3542=LINE('',#20806,#4781);
#3543=LINE('',#20808,#4782);
#3544=LINE('',#20810,#4783);
#3545=LINE('',#20812,#4784);
#3546=LINE('',#20816,#4785);
#3547=LINE('',#20818,#4786);
#3548=LINE('',#20819,#4787);
#3549=LINE('',#20823,#4788);
#3550=LINE('',#20824,#4789);
#3551=LINE('',#20825,#4790);
#3552=LINE('',#20829,#4791);
#3553=LINE('',#20831,#4792);
#3554=LINE('',#20832,#4793);
#3555=LINE('',#20836,#4794);
#3556=LINE('',#20837,#4795);
#3557=LINE('',#20838,#4796);
#3558=LINE('',#20842,#4797);
#3559=LINE('',#20843,#4798);
#3560=LINE('',#20845,#4799);
#3561=LINE('',#20846,#4800);
#3562=LINE('',#20848,#4801);
#3563=LINE('',#20849,#4802);
#3564=LINE('',#20853,#4803);
#3565=LINE('',#20854,#4804);
#3566=LINE('',#20856,#4805);
#3567=LINE('',#20857,#4806);
#3568=LINE('',#20859,#4807);
#3569=LINE('',#20862,#4808);
#3570=LINE('',#20863,#4809);
#3571=LINE('',#20866,#4810);
#3572=LINE('',#20868,#4811);
#3573=LINE('',#20869,#4812);
#3574=LINE('',#20873,#4813);
#3575=LINE('',#20875,#4814);
#3576=LINE('',#20876,#4815);
#3577=LINE('',#20880,#4816);
#3578=LINE('',#20881,#4817);
#3579=LINE('',#20882,#4818);
#3580=LINE('',#20886,#4819);
#3581=LINE('',#20888,#4820);
#3582=LINE('',#20889,#4821);
#3583=LINE('',#20893,#4822);
#3584=LINE('',#20894,#4823);
#3585=LINE('',#20895,#4824);
#3586=LINE('',#20899,#4825);
#3587=LINE('',#20900,#4826);
#3588=LINE('',#20902,#4827);
#3589=LINE('',#20903,#4828);
#3590=LINE('',#20905,#4829);
#3591=LINE('',#20906,#4830);
#3592=LINE('',#20910,#4831);
#3593=LINE('',#20911,#4832);
#3594=LINE('',#20913,#4833);
#3595=LINE('',#20914,#4834);
#3596=LINE('',#20916,#4835);
#3597=LINE('',#20919,#4836);
#3598=LINE('',#20920,#4837);
#3599=LINE('',#20923,#4838);
#3600=LINE('',#20925,#4839);
#3601=LINE('',#20926,#4840);
#3602=LINE('',#20929,#4841);
#3603=LINE('',#20931,#4842);
#3604=LINE('',#20933,#4843);
#3605=LINE('',#20934,#4844);
#3606=LINE('',#20937,#4845);
#3607=LINE('',#20938,#4846);
#3608=LINE('',#20941,#4847);
#3609=LINE('',#20943,#4848);
#3610=LINE('',#20944,#4849);
#3611=LINE('',#20948,#4850);
#3612=LINE('',#20950,#4851);
#3613=LINE('',#20952,#4852);
#3614=LINE('',#20953,#4853);
#3615=LINE('',#20956,#4854);
#3616=LINE('',#20958,#4855);
#3617=LINE('',#20959,#4856);
#3618=LINE('',#20962,#4857);
#3619=LINE('',#20964,#4858);
#3620=LINE('',#20965,#4859);
#3621=LINE('',#20968,#4860);
#3622=LINE('',#20969,#4861);
#3623=LINE('',#20972,#4862);
#3624=LINE('',#20974,#4863);
#3625=LINE('',#20975,#4864);
#3626=LINE('',#20977,#4865);
#3627=LINE('',#20978,#4866);
#3628=LINE('',#20982,#4867);
#3629=LINE('',#20984,#4868);
#3630=LINE('',#20988,#4869);
#3631=LINE('',#20989,#4870);
#3632=LINE('',#20991,#4871);
#3633=LINE('',#20993,#4872);
#3634=LINE('',#20994,#4873);
#3635=LINE('',#20996,#4874);
#3636=LINE('',#20998,#4875);
#3637=LINE('',#20999,#4876);
#3638=LINE('',#21001,#4877);
#3639=LINE('',#21003,#4878);
#3640=LINE('',#21005,#4879);
#3641=LINE('',#21007,#4880);
#3642=LINE('',#21010,#4881);
#3643=LINE('',#21013,#4882);
#3644=LINE('',#21015,#4883);
#3645=LINE('',#21016,#4884);
#3646=LINE('',#21020,#4885);
#3647=LINE('',#21026,#4886);
#3648=LINE('',#21027,#4887);
#3649=LINE('',#21028,#4888);
#3650=LINE('',#21032,#4889);
#3651=LINE('',#21038,#4890);
#3652=LINE('',#21039,#4891);
#3653=LINE('',#21040,#4892);
#3654=LINE('',#21044,#4893);
#3655=LINE('',#21050,#4894);
#3656=LINE('',#21051,#4895);
#3657=LINE('',#21052,#4896);
#3658=LINE('',#21058,#4897);
#3659=LINE('',#21061,#4898);
#3660=LINE('',#21064,#4899);
#3661=LINE('',#21065,#4900);
#3662=LINE('',#21089,#4901);
#3663=LINE('',#21090,#4902);
#3664=LINE('',#21093,#4903);
#3665=LINE('',#21094,#4904);
#3666=LINE('',#21096,#4905);
#3667=LINE('',#21097,#4906);
#3668=LINE('',#21100,#4907);
#3669=LINE('',#21101,#4908);
#3670=LINE('',#21106,#4909);
#3671=LINE('',#21111,#4910);
#3672=LINE('',#21112,#4911);
#3673=LINE('',#21113,#4912);
#3674=LINE('',#21118,#4913);
#3675=LINE('',#21122,#4914);
#3676=LINE('',#21123,#4915);
#3677=LINE('',#21124,#4916);
#3678=LINE('',#21127,#4917);
#3679=LINE('',#21131,#4918);
#3680=LINE('',#21132,#4919);
#3681=LINE('',#21135,#4920);
#3682=LINE('',#21138,#4921);
#3683=LINE('',#21139,#4922);
#3684=LINE('',#21141,#4923);
#3685=LINE('',#21143,#4924);
#3686=LINE('',#21145,#4925);
#3687=LINE('',#21147,#4926);
#3688=LINE('',#21148,#4927);
#3689=LINE('',#21150,#4928);
#3690=LINE('',#21152,#4929);
#3691=LINE('',#21154,#4930);
#3692=LINE('',#21156,#4931);
#3693=LINE('',#21175,#4932);
#3694=LINE('',#21178,#4933);
#3695=LINE('',#21206,#4934);
#3696=LINE('',#21208,#4935);
#3697=LINE('',#21217,#4936);
#3698=LINE('',#21222,#4937);
#3699=LINE('',#21265,#4938);
#3700=LINE('',#21292,#4939);
#3701=LINE('',#21294,#4940);
#3702=LINE('',#21306,#4941);
#3703=LINE('',#21309,#4942);
#3704=LINE('',#21352,#4943);
#3705=LINE('',#21356,#4944);
#3706=LINE('',#21360,#4945);
#3707=LINE('',#21365,#4946);
#3708=LINE('',#21368,#4947);
#3709=LINE('',#21369,#4948);
#3710=LINE('',#21373,#4949);
#3711=LINE('',#21375,#4950);
#3712=LINE('',#21378,#4951);
#3713=LINE('',#21380,#4952);
#3714=LINE('',#21383,#4953);
#3715=LINE('',#21391,#4954);
#3716=LINE('',#21396,#4955);
#3717=LINE('',#21400,#4956);
#3718=LINE('',#21404,#4957);
#3719=LINE('',#21408,#4958);
#3720=LINE('',#21412,#4959);
#3721=LINE('',#21421,#4960);
#3722=LINE('',#21425,#4961);
#3723=LINE('',#21429,#4962);
#3724=LINE('',#21433,#4963);
#3725=LINE('',#21437,#4964);
#3726=LINE('',#21445,#4965);
#3727=LINE('',#21447,#4966);
#3728=LINE('',#21448,#4967);
#3729=LINE('',#21452,#4968);
#3730=LINE('',#21455,#4969);
#3731=LINE('',#21456,#4970);
#3732=LINE('',#21460,#4971);
#3733=LINE('',#21463,#4972);
#3734=LINE('',#21464,#4973);
#3735=LINE('',#21468,#4974);
#3736=LINE('',#21471,#4975);
#3737=LINE('',#21472,#4976);
#3738=LINE('',#21477,#4977);
#3739=LINE('',#21480,#4978);
#3740=LINE('',#21483,#4979);
#3741=LINE('',#21484,#4980);
#3742=LINE('',#21487,#4981);
#3743=LINE('',#21491,#4982);
#3744=LINE('',#21492,#4983);
#3745=LINE('',#21495,#4984);
#3746=LINE('',#21497,#4985);
#3747=LINE('',#21499,#4986);
#3748=LINE('',#21500,#4987);
#3749=LINE('',#21503,#4988);
#3750=LINE('',#21507,#4989);
#3751=LINE('',#21508,#4990);
#3752=LINE('',#21511,#4991);
#3753=LINE('',#21515,#4992);
#3754=LINE('',#21516,#4993);
#3755=LINE('',#21520,#4994);
#3756=LINE('',#21526,#4995);
#3757=LINE('',#21527,#4996);
#3758=LINE('',#21528,#4997);
#3759=LINE('',#21534,#4998);
#3760=LINE('',#21537,#4999);
#3761=LINE('',#21540,#5000);
#3762=LINE('',#21541,#5001);
#3763=LINE('',#21544,#5002);
#3764=LINE('',#21548,#5003);
#3765=LINE('',#21549,#5004);
#3766=LINE('',#21551,#5005);
#3767=LINE('',#21553,#5006);
#3768=LINE('',#21554,#5007);
#3769=LINE('',#21556,#5008);
#3770=LINE('',#21558,#5009);
#3771=LINE('',#21560,#5010);
#3772=LINE('',#21563,#5011);
#3773=LINE('',#21564,#5012);
#3774=LINE('',#21567,#5013);
#3775=LINE('',#21571,#5014);
#3776=LINE('',#21572,#5015);
#3777=LINE('',#21576,#5016);
#3778=LINE('',#21577,#5017);
#3779=LINE('',#21579,#5018);
#3780=LINE('',#21583,#5019);
#3781=LINE('',#21585,#5020);
#3782=LINE('',#21587,#5021);
#3783=LINE('',#21589,#5022);
#3784=LINE('',#21595,#5023);
#3785=LINE('',#21597,#5024);
#3786=LINE('',#21599,#5025);
#3787=LINE('',#21600,#5026);
#3788=LINE('',#21603,#5027);
#3789=LINE('',#21605,#5028);
#3790=LINE('',#21606,#5029);
#3791=LINE('',#21609,#5030);
#3792=LINE('',#21611,#5031);
#3793=LINE('',#21612,#5032);
#3794=LINE('',#21614,#5033);
#3795=LINE('',#21615,#5034);
#3796=LINE('',#21620,#5035);
#3797=LINE('',#21622,#5036);
#3798=LINE('',#21624,#5037);
#3799=LINE('',#21625,#5038);
#3800=LINE('',#21628,#5039);
#3801=LINE('',#21630,#5040);
#3802=LINE('',#21631,#5041);
#3803=LINE('',#21634,#5042);
#3804=LINE('',#21636,#5043);
#3805=LINE('',#21637,#5044);
#3806=LINE('',#21639,#5045);
#3807=LINE('',#21640,#5046);
#3808=LINE('',#21645,#5047);
#3809=LINE('',#21647,#5048);
#3810=LINE('',#21649,#5049);
#3811=LINE('',#21650,#5050);
#3812=LINE('',#21653,#5051);
#3813=LINE('',#21655,#5052);
#3814=LINE('',#21656,#5053);
#3815=LINE('',#21659,#5054);
#3816=LINE('',#21661,#5055);
#3817=LINE('',#21662,#5056);
#3818=LINE('',#21664,#5057);
#3819=LINE('',#21665,#5058);
#3820=LINE('',#21670,#5059);
#3821=LINE('',#21672,#5060);
#3822=LINE('',#21674,#5061);
#3823=LINE('',#21675,#5062);
#3824=LINE('',#21678,#5063);
#3825=LINE('',#21680,#5064);
#3826=LINE('',#21681,#5065);
#3827=LINE('',#21684,#5066);
#3828=LINE('',#21686,#5067);
#3829=LINE('',#21687,#5068);
#3830=LINE('',#21689,#5069);
#3831=LINE('',#21690,#5070);
#3832=LINE('',#21697,#5071);
#3833=LINE('',#21699,#5072);
#3834=LINE('',#21700,#5073);
#3835=LINE('',#21704,#5074);
#3836=LINE('',#21706,#5075);
#3837=LINE('',#21707,#5076);
#3838=LINE('',#21711,#5077);
#3839=LINE('',#21713,#5078);
#3840=LINE('',#21714,#5079);
#3841=LINE('',#21718,#5080);
#3842=LINE('',#21720,#5081);
#3843=LINE('',#21721,#5082);
#3844=LINE('',#21725,#5083);
#3845=LINE('',#21727,#5084);
#3846=LINE('',#21728,#5085);
#3847=LINE('',#21732,#5086);
#3848=LINE('',#21734,#5087);
#3849=LINE('',#21735,#5088);
#3850=LINE('',#21739,#5089);
#3851=LINE('',#21741,#5090);
#3852=LINE('',#21742,#5091);
#3853=LINE('',#21744,#5092);
#3854=LINE('',#21745,#5093);
#3855=LINE('',#21749,#5094);
#3856=LINE('',#21751,#5095);
#3857=LINE('',#21752,#5096);
#3858=LINE('',#21754,#5097);
#3859=LINE('',#21755,#5098);
#3860=LINE('',#21757,#5099);
#3861=LINE('',#21758,#5100);
#3862=LINE('',#21760,#5101);
#3863=LINE('',#21761,#5102);
#3864=LINE('',#21763,#5103);
#3865=LINE('',#21764,#5104);
#3866=LINE('',#21766,#5105);
#3867=LINE('',#21767,#5106);
#3868=LINE('',#21769,#5107);
#3869=LINE('',#21770,#5108);
#3870=LINE('',#21772,#5109);
#3871=LINE('',#21773,#5110);
#3872=LINE('',#21775,#5111);
#3873=LINE('',#21776,#5112);
#3874=LINE('',#21778,#5113);
#3875=LINE('',#21779,#5114);
#3876=LINE('',#21781,#5115);
#3877=LINE('',#21782,#5116);
#3878=LINE('',#21784,#5117);
#3879=LINE('',#21785,#5118);
#3880=LINE('',#21797,#5119);
#3881=LINE('',#21802,#5120);
#3882=LINE('',#21826,#5121);
#3883=LINE('',#21874,#5122);
#3884=LINE('',#21922,#5123);
#3885=LINE('',#21976,#5124);
#3886=LINE('',#22024,#5125);
#3887=LINE('',#22072,#5126);
#3888=LINE('',#22126,#5127);
#3889=LINE('',#22174,#5128);
#3890=LINE('',#22222,#5129);
#3891=LINE('',#22270,#5130);
#3892=LINE('',#22324,#5131);
#3893=LINE('',#22372,#5132);
#3894=LINE('',#22420,#5133);
#3895=LINE('',#22474,#5134);
#3896=LINE('',#22522,#5135);
#3897=LINE('',#22570,#5136);
#3898=LINE('',#22624,#5137);
#3899=LINE('',#22672,#5138);
#3900=LINE('',#22720,#5139);
#3901=LINE('',#22774,#5140);
#3902=LINE('',#22822,#5141);
#3903=LINE('',#22870,#5142);
#3904=LINE('',#22924,#5143);
#3905=LINE('',#22972,#5144);
#3906=LINE('',#23020,#5145);
#3907=LINE('',#23074,#5146);
#3908=LINE('',#23122,#5147);
#3909=LINE('',#23170,#5148);
#3910=LINE('',#23194,#5149);
#3911=LINE('',#23218,#5150);
#3912=LINE('',#23243,#5151);
#3913=LINE('',#23268,#5152);
#3914=LINE('',#23292,#5153);
#3915=LINE('',#23317,#5154);
#3916=LINE('',#23342,#5155);
#3917=LINE('',#23366,#5156);
#3918=LINE('',#23391,#5157);
#3919=LINE('',#23416,#5158);
#3920=LINE('',#23440,#5159);
#3921=LINE('',#23465,#5160);
#3922=LINE('',#23490,#5161);
#3923=LINE('',#23514,#5162);
#3924=LINE('',#23539,#5163);
#3925=LINE('',#23564,#5164);
#3926=LINE('',#23588,#5165);
#3927=LINE('',#23613,#5166);
#3928=LINE('',#23638,#5167);
#3929=LINE('',#23662,#5168);
#3930=LINE('',#23686,#5169);
#3931=LINE('',#23711,#5170);
#3932=LINE('',#23736,#5171);
#3933=LINE('',#23760,#5172);
#3934=LINE('',#23785,#5173);
#3935=LINE('',#23810,#5174);
#3936=LINE('',#23836,#5175);
#3937=LINE('',#23937,#5176);
#3938=LINE('',#23940,#5177);
#3939=LINE('',#23942,#5178);
#3940=LINE('',#23945,#5179);
#3941=LINE('',#23947,#5180);
#3942=LINE('',#23950,#5181);
#3943=LINE('',#23952,#5182);
#3944=LINE('',#23955,#5183);
#3945=LINE('',#23957,#5184);
#3946=LINE('',#23960,#5185);
#3947=LINE('',#23962,#5186);
#3948=LINE('',#23965,#5187);
#3949=LINE('',#23967,#5188);
#3950=LINE('',#23970,#5189);
#3951=LINE('',#23972,#5190);
#3952=LINE('',#23975,#5191);
#3953=LINE('',#23977,#5192);
#3954=LINE('',#23980,#5193);
#3955=LINE('',#23982,#5194);
#3956=LINE('',#23985,#5195);
#3957=LINE('',#23987,#5196);
#3958=LINE('',#23990,#5197);
#3959=LINE('',#23992,#5198);
#3960=LINE('',#23995,#5199);
#3961=LINE('',#23997,#5200);
#3962=LINE('',#24000,#5201);
#3963=LINE('',#24002,#5202);
#3964=LINE('',#24005,#5203);
#3965=LINE('',#24007,#5204);
#3966=LINE('',#24010,#5205);
#3967=LINE('',#24012,#5206);
#3968=LINE('',#24015,#5207);
#3969=LINE('',#24017,#5208);
#3970=LINE('',#24020,#5209);
#3971=LINE('',#24022,#5210);
#3972=LINE('',#24025,#5211);
#3973=LINE('',#24027,#5212);
#3974=LINE('',#24030,#5213);
#3975=LINE('',#24032,#5214);
#3976=LINE('',#24035,#5215);
#3977=LINE('',#24037,#5216);
#3978=LINE('',#24040,#5217);
#3979=LINE('',#24042,#5218);
#3980=LINE('',#24045,#5219);
#3981=LINE('',#24047,#5220);
#3982=LINE('',#24050,#5221);
#3983=LINE('',#24052,#5222);
#3984=LINE('',#24055,#5223);
#3985=LINE('',#24057,#5224);
#3986=LINE('',#25927,#5225);
#3987=LINE('',#25929,#5226);
#3988=LINE('',#25930,#5227);
#3989=LINE('',#25932,#5228);
#3990=LINE('',#25934,#5229);
#3991=LINE('',#25938,#5230);
#3992=LINE('',#25940,#5231);
#3993=LINE('',#25941,#5232);
#3994=LINE('',#25943,#5233);
#3995=LINE('',#25945,#5234);
#3996=LINE('',#25949,#5235);
#3997=LINE('',#25951,#5236);
#3998=LINE('',#25952,#5237);
#3999=LINE('',#25954,#5238);
#4000=LINE('',#25956,#5239);
#4001=LINE('',#25960,#5240);
#4002=LINE('',#25962,#5241);
#4003=LINE('',#25963,#5242);
#4004=LINE('',#25965,#5243);
#4005=LINE('',#25967,#5244);
#4006=LINE('',#25971,#5245);
#4007=LINE('',#25973,#5246);
#4008=LINE('',#25974,#5247);
#4009=LINE('',#25976,#5248);
#4010=LINE('',#25978,#5249);
#4011=LINE('',#25982,#5250);
#4012=LINE('',#25984,#5251);
#4013=LINE('',#25985,#5252);
#4014=LINE('',#25987,#5253);
#4015=LINE('',#25989,#5254);
#4016=LINE('',#25993,#5255);
#4017=LINE('',#25995,#5256);
#4018=LINE('',#25996,#5257);
#4019=LINE('',#25998,#5258);
#4020=LINE('',#26000,#5259);
#4021=LINE('',#26004,#5260);
#4022=LINE('',#26006,#5261);
#4023=LINE('',#26007,#5262);
#4024=LINE('',#26009,#5263);
#4025=LINE('',#26011,#5264);
#4026=LINE('',#26015,#5265);
#4027=LINE('',#26017,#5266);
#4028=LINE('',#26018,#5267);
#4029=LINE('',#26020,#5268);
#4030=LINE('',#26022,#5269);
#4031=LINE('',#26026,#5270);
#4032=LINE('',#26028,#5271);
#4033=LINE('',#26029,#5272);
#4034=LINE('',#26031,#5273);
#4035=LINE('',#26033,#5274);
#4036=LINE('',#26037,#5275);
#4037=LINE('',#26039,#5276);
#4038=LINE('',#26040,#5277);
#4039=LINE('',#26042,#5278);
#4040=LINE('',#26044,#5279);
#4041=LINE('',#26048,#5280);
#4042=LINE('',#26050,#5281);
#4043=LINE('',#26051,#5282);
#4044=LINE('',#26053,#5283);
#4045=LINE('',#26055,#5284);
#4046=LINE('',#26059,#5285);
#4047=LINE('',#26061,#5286);
#4048=LINE('',#26062,#5287);
#4049=LINE('',#26064,#5288);
#4050=LINE('',#26066,#5289);
#4051=LINE('',#26070,#5290);
#4052=LINE('',#26072,#5291);
#4053=LINE('',#26073,#5292);
#4054=LINE('',#26075,#5293);
#4055=LINE('',#26077,#5294);
#4056=LINE('',#26081,#5295);
#4057=LINE('',#26083,#5296);
#4058=LINE('',#26084,#5297);
#4059=LINE('',#26086,#5298);
#4060=LINE('',#26088,#5299);
#4061=LINE('',#26092,#5300);
#4062=LINE('',#26094,#5301);
#4063=LINE('',#26095,#5302);
#4064=LINE('',#26097,#5303);
#4065=LINE('',#26099,#5304);
#4066=LINE('',#26103,#5305);
#4067=LINE('',#26105,#5306);
#4068=LINE('',#26106,#5307);
#4069=LINE('',#26108,#5308);
#4070=LINE('',#26110,#5309);
#4071=LINE('',#26114,#5310);
#4072=LINE('',#26116,#5311);
#4073=LINE('',#26117,#5312);
#4074=LINE('',#26119,#5313);
#4075=LINE('',#26121,#5314);
#4076=LINE('',#26125,#5315);
#4077=LINE('',#26127,#5316);
#4078=LINE('',#26128,#5317);
#4079=LINE('',#26130,#5318);
#4080=LINE('',#26132,#5319);
#4081=LINE('',#26136,#5320);
#4082=LINE('',#26138,#5321);
#4083=LINE('',#26139,#5322);
#4084=LINE('',#26141,#5323);
#4085=LINE('',#26143,#5324);
#4086=LINE('',#26147,#5325);
#4087=LINE('',#26149,#5326);
#4088=LINE('',#26150,#5327);
#4089=LINE('',#26152,#5328);
#4090=LINE('',#26154,#5329);
#4091=LINE('',#26158,#5330);
#4092=LINE('',#26160,#5331);
#4093=LINE('',#26161,#5332);
#4094=LINE('',#26163,#5333);
#4095=LINE('',#26165,#5334);
#4096=LINE('',#26169,#5335);
#4097=LINE('',#26171,#5336);
#4098=LINE('',#26172,#5337);
#4099=LINE('',#26174,#5338);
#4100=LINE('',#26176,#5339);
#4101=LINE('',#26180,#5340);
#4102=LINE('',#26182,#5341);
#4103=LINE('',#26183,#5342);
#4104=LINE('',#26185,#5343);
#4105=LINE('',#26187,#5344);
#4106=LINE('',#26193,#5345);
#4107=LINE('',#26198,#5346);
#4108=LINE('',#26204,#5347);
#4109=LINE('',#26214,#5348);
#4110=LINE('',#26218,#5349);
#4111=LINE('',#26230,#5350);
#4112=LINE('',#26232,#5351);
#4113=LINE('',#26233,#5352);
#4114=LINE('',#26245,#5353);
#4115=LINE('',#26249,#5354);
#4116=LINE('',#26258,#5355);
#4117=LINE('',#26262,#5356);
#4118=LINE('',#26266,#5357);
#4119=LINE('',#26270,#5358);
#4120=LINE('',#26274,#5359);
#4121=LINE('',#26278,#5360);
#4122=LINE('',#26282,#5361);
#4123=LINE('',#26286,#5362);
#4124=LINE('',#26290,#5363);
#4125=LINE('',#26294,#5364);
#4126=LINE('',#26298,#5365);
#4127=LINE('',#26302,#5366);
#4128=LINE('',#26306,#5367);
#4129=LINE('',#26310,#5368);
#4130=LINE('',#26315,#5369);
#4131=LINE('',#26319,#5370);
#4132=LINE('',#26323,#5371);
#4133=LINE('',#26327,#5372);
#4134=LINE('',#26331,#5373);
#4135=LINE('',#26335,#5374);
#4136=LINE('',#26339,#5375);
#4137=LINE('',#26343,#5376);
#4138=LINE('',#26347,#5377);
#4139=LINE('',#26351,#5378);
#4140=LINE('',#26355,#5379);
#4141=LINE('',#26359,#5380);
#4142=LINE('',#26363,#5381);
#4143=LINE('',#26367,#5382);
#4144=LINE('',#26371,#5383);
#4145=LINE('',#26374,#5384);
#4146=LINE('',#26377,#5385);
#4147=LINE('',#26657,#5386);
#4148=LINE('',#26658,#5387);
#4149=LINE('',#26661,#5388);
#4150=LINE('',#26662,#5389);
#4151=LINE('',#26665,#5390);
#4152=LINE('',#26666,#5391);
#4153=LINE('',#26669,#5392);
#4154=LINE('',#26670,#5393);
#4155=LINE('',#26673,#5394);
#4156=LINE('',#26674,#5395);
#4157=LINE('',#26677,#5396);
#4158=LINE('',#26678,#5397);
#4159=LINE('',#26681,#5398);
#4160=LINE('',#26682,#5399);
#4161=LINE('',#26685,#5400);
#4162=LINE('',#26686,#5401);
#4163=LINE('',#26689,#5402);
#4164=LINE('',#26690,#5403);
#4165=LINE('',#26693,#5404);
#4166=LINE('',#26694,#5405);
#4167=LINE('',#26697,#5406);
#4168=LINE('',#26698,#5407);
#4169=LINE('',#26701,#5408);
#4170=LINE('',#26702,#5409);
#4171=LINE('',#26705,#5410);
#4172=LINE('',#26706,#5411);
#4173=LINE('',#26709,#5412);
#4174=LINE('',#26710,#5413);
#4175=LINE('',#26713,#5414);
#4176=LINE('',#26714,#5415);
#4177=LINE('',#26717,#5416);
#4178=LINE('',#26718,#5417);
#4179=LINE('',#26721,#5418);
#4180=LINE('',#26722,#5419);
#4181=LINE('',#26725,#5420);
#4182=LINE('',#26726,#5421);
#4183=LINE('',#26729,#5422);
#4184=LINE('',#26730,#5423);
#4185=LINE('',#26733,#5424);
#4186=LINE('',#26734,#5425);
#4187=LINE('',#26737,#5426);
#4188=LINE('',#26738,#5427);
#4189=LINE('',#26741,#5428);
#4190=LINE('',#26742,#5429);
#4191=LINE('',#26745,#5430);
#4192=LINE('',#26746,#5431);
#4193=LINE('',#26749,#5432);
#4194=LINE('',#26750,#5433);
#4195=LINE('',#26753,#5434);
#4196=LINE('',#26754,#5435);
#4197=LINE('',#26757,#5436);
#4198=LINE('',#26758,#5437);
#4199=LINE('',#26761,#5438);
#4200=LINE('',#26762,#5439);
#4201=LINE('',#26765,#5440);
#4202=LINE('',#26766,#5441);
#4203=LINE('',#26769,#5442);
#4204=LINE('',#26770,#5443);
#4205=LINE('',#26853,#5444);
#4206=LINE('',#26854,#5445);
#4207=LINE('',#26857,#5446);
#4208=LINE('',#26858,#5447);
#4209=LINE('',#26863,#5448);
#4210=LINE('',#26868,#5449);
#4211=LINE('',#26870,#5450);
#4212=LINE('',#26872,#5451);
#4213=LINE('',#26874,#5452);
#4214=LINE('',#26876,#5453);
#4215=LINE('',#26877,#5454);
#4216=LINE('',#26881,#5455);
#4217=LINE('',#26883,#5456);
#4218=LINE('',#26885,#5457);
#4219=LINE('',#26886,#5458);
#4220=LINE('',#26889,#5459);
#4221=LINE('',#26891,#5460);
#4222=LINE('',#26892,#5461);
#4223=LINE('',#26896,#5462);
#4224=LINE('',#26898,#5463);
#4225=LINE('',#26900,#5464);
#4226=LINE('',#26901,#5465);
#4227=LINE('',#26904,#5466);
#4228=LINE('',#26906,#5467);
#4229=LINE('',#26907,#5468);
#4230=LINE('',#26909,#5469);
#4231=LINE('',#26910,#5470);
#4232=LINE('',#26912,#5471);
#4233=LINE('',#26913,#5472);
#4234=LINE('',#26915,#5473);
#4235=LINE('',#26916,#5474);
#4236=LINE('',#26918,#5475);
#4237=LINE('',#26920,#5476);
#4238=LINE('',#26925,#5477);
#4239=LINE('',#26927,#5478);
#4240=LINE('',#26976,#5479);
#4241=LINE('',#26981,#5480);
#4242=LINE('',#27005,#5481);
#4243=LINE('',#27053,#5482);
#4244=LINE('',#27101,#5483);
#4245=LINE('',#27155,#5484);
#4246=LINE('',#27203,#5485);
#4247=LINE('',#27251,#5486);
#4248=LINE('',#27299,#5487);
#4249=LINE('',#27353,#5488);
#4250=LINE('',#27401,#5489);
#4251=LINE('',#27449,#5490);
#4252=LINE('',#27503,#5491);
#4253=LINE('',#27551,#5492);
#4254=LINE('',#27599,#5493);
#4255=LINE('',#27653,#5494);
#4256=LINE('',#27701,#5495);
#4257=LINE('',#27749,#5496);
#4258=LINE('',#27797,#5497);
#4259=LINE('',#27848,#5498);
#4260=LINE('',#27896,#5499);
#4261=LINE('',#27944,#5500);
#4262=LINE('',#27998,#5501);
#4263=LINE('',#28046,#5502);
#4264=LINE('',#28094,#5503);
#4265=LINE('',#28116,#5504);
#4266=LINE('',#28140,#5505);
#4267=LINE('',#28165,#5506);
#4268=LINE('',#28190,#5507);
#4269=LINE('',#28214,#5508);
#4270=LINE('',#28239,#5509);
#4271=LINE('',#28264,#5510);
#4272=LINE('',#28288,#5511);
#4273=LINE('',#28312,#5512);
#4274=LINE('',#28337,#5513);
#4275=LINE('',#28362,#5514);
#4276=LINE('',#28386,#5515);
#4277=LINE('',#28411,#5516);
#4278=LINE('',#28436,#5517);
#4279=LINE('',#28460,#5518);
#4280=LINE('',#28485,#5519);
#4281=LINE('',#28510,#5520);
#4282=LINE('',#28534,#5521);
#4283=LINE('',#28558,#5522);
#4284=LINE('',#28583,#5523);
#4285=LINE('',#28608,#5524);
#4286=LINE('',#30187,#5525);
#4287=LINE('',#30211,#5526);
#4288=LINE('',#30222,#5527);
#4289=LINE('',#30224,#5528);
#4290=LINE('',#30225,#5529);
#4291=LINE('',#30228,#5530);
#4292=LINE('',#30229,#5531);
#4293=LINE('',#30232,#5532);
#4294=LINE('',#30233,#5533);
#4295=LINE('',#30236,#5534);
#4296=LINE('',#30237,#5535);
#4297=LINE('',#30240,#5536);
#4298=LINE('',#30241,#5537);
#4299=LINE('',#30243,#5538);
#4300=LINE('',#30250,#5539);
#4301=LINE('',#30274,#5540);
#4302=LINE('',#30322,#5541);
#4303=LINE('',#30370,#5542);
#4304=LINE('',#30424,#5543);
#4305=LINE('',#30472,#5544);
#4306=LINE('',#30520,#5545);
#4307=LINE('',#30568,#5546);
#4308=LINE('',#30622,#5547);
#4309=LINE('',#30670,#5548);
#4310=LINE('',#30718,#5549);
#4311=LINE('',#30772,#5550);
#4312=LINE('',#30820,#5551);
#4313=LINE('',#30868,#5552);
#4314=LINE('',#30922,#5553);
#4315=LINE('',#30970,#5554);
#4316=LINE('',#31018,#5555);
#4317=LINE('',#31066,#5556);
#4318=LINE('',#31120,#5557);
#4319=LINE('',#31168,#5558);
#4320=LINE('',#31216,#5559);
#4321=LINE('',#31270,#5560);
#4322=LINE('',#31318,#5561);
#4323=LINE('',#31366,#5562);
#4324=LINE('',#31420,#5563);
#4325=LINE('',#31468,#5564);
#4326=LINE('',#31516,#5565);
#4327=LINE('',#31570,#5566);
#4328=LINE('',#31618,#5567);
#4329=LINE('',#31636,#5568);
#4330=LINE('',#31660,#5569);
#4331=LINE('',#31685,#5570);
#4332=LINE('',#31710,#5571);
#4333=LINE('',#31734,#5572);
#4334=LINE('',#31759,#5573);
#4335=LINE('',#31784,#5574);
#4336=LINE('',#31808,#5575);
#4337=LINE('',#31833,#5576);
#4338=LINE('',#31858,#5577);
#4339=LINE('',#31882,#5578);
#4340=LINE('',#31907,#5579);
#4341=LINE('',#31932,#5580);
#4342=LINE('',#31956,#5581);
#4343=LINE('',#31980,#5582);
#4344=LINE('',#32005,#5583);
#4345=LINE('',#32030,#5584);
#4346=LINE('',#32054,#5585);
#4347=LINE('',#32079,#5586);
#4348=LINE('',#32104,#5587);
#4349=LINE('',#32128,#5588);
#4350=LINE('',#32153,#5589);
#4351=LINE('',#32178,#5590);
#4352=LINE('',#32202,#5591);
#4353=LINE('',#32226,#5592);
#4354=LINE('',#32251,#5593);
#4355=LINE('',#32276,#5594);
#4356=LINE('',#34164,#5595);
#4357=LINE('',#34176,#5596);
#4358=LINE('',#34178,#5597);
#4359=LINE('',#34179,#5598);
#4360=LINE('',#34189,#5599);
#4361=LINE('',#34190,#5600);
#4362=LINE('',#34200,#5601);
#4363=LINE('',#34201,#5602);
#4364=LINE('',#34211,#5603);
#4365=LINE('',#34212,#5604);
#4366=LINE('',#34222,#5605);
#4367=LINE('',#34223,#5606);
#4368=LINE('',#34231,#5607);
#4369=LINE('',#34237,#5608);
#4370=LINE('',#34247,#5609);
#4371=LINE('',#34284,#5610);
#4372=LINE('',#34290,#5611);
#4373=LINE('',#34297,#5612);
#4374=LINE('',#34303,#5613);
#4375=LINE('',#34312,#5614);
#4376=LINE('',#34317,#5615);
#4377=LINE('',#34324,#5616);
#4378=LINE('',#34350,#5617);
#4379=LINE('',#34379,#5618);
#4380=LINE('',#34383,#5619);
#4381=LINE('',#34391,#5620);
#4382=LINE('',#34395,#5621);
#4383=LINE('',#34400,#5622);
#4384=LINE('',#34406,#5623);
#4385=LINE('',#34409,#5624);
#4386=LINE('',#34444,#5625);
#4387=LINE('',#34446,#5626);
#4388=LINE('',#34448,#5627);
#4389=LINE('',#34450,#5628);
#4390=LINE('',#34452,#5629);
#4391=LINE('',#34454,#5630);
#4392=LINE('',#34461,#5631);
#4393=LINE('',#34485,#5632);
#4394=LINE('',#34533,#5633);
#4395=LINE('',#34581,#5634);
#4396=LINE('',#34632,#5635);
#4397=LINE('',#34683,#5636);
#4398=LINE('',#34731,#5637);
#4399=LINE('',#34779,#5638);
#4400=LINE('',#34833,#5639);
#4401=LINE('',#34881,#5640);
#4402=LINE('',#34929,#5641);
#4403=LINE('',#34983,#5642);
#4404=LINE('',#35031,#5643);
#4405=LINE('',#35079,#5644);
#4406=LINE('',#35127,#5645);
#4407=LINE('',#35181,#5646);
#4408=LINE('',#35229,#5647);
#4409=LINE('',#35277,#5648);
#4410=LINE('',#35330,#5649);
#4411=LINE('',#35351,#5650);
#4412=LINE('',#35376,#5651);
#4413=LINE('',#35400,#5652);
#4414=LINE('',#35425,#5653);
#4415=LINE('',#35450,#5654);
#4416=LINE('',#35474,#5655);
#4417=LINE('',#35498,#5656);
#4418=LINE('',#35523,#5657);
#4419=LINE('',#35548,#5658);
#4420=LINE('',#35572,#5659);
#4421=LINE('',#35597,#5660);
#4422=LINE('',#35622,#5661);
#4423=LINE('',#35646,#5662);
#4424=LINE('',#35671,#5663);
#4425=LINE('',#35695,#5664);
#4426=LINE('',#35720,#5665);
#4427=LINE('',#37014,#5666);
#4428=LINE('',#37026,#5667);
#4429=LINE('',#37028,#5668);
#4430=LINE('',#37029,#5669);
#4431=LINE('',#37039,#5670);
#4432=LINE('',#37040,#5671);
#4433=LINE('',#37050,#5672);
#4434=LINE('',#37051,#5673);
#4435=LINE('',#37061,#5674);
#4436=LINE('',#37062,#5675);
#4437=LINE('',#37072,#5676);
#4438=LINE('',#37073,#5677);
#4439=LINE('',#37081,#5678);
#4440=LINE('',#37087,#5679);
#4441=LINE('',#37097,#5680);
#4442=VECTOR('',#16131,10.);
#4443=VECTOR('',#16132,10.);
#4444=VECTOR('',#16133,10.);
#4445=VECTOR('',#16134,10.);
#4446=VECTOR('',#16137,10.);
#4447=VECTOR('',#16138,10.);
#4448=VECTOR('',#16139,10.);
#4449=VECTOR('',#16150,10.);
#4450=VECTOR('',#16153,10.);
#4451=VECTOR('',#16154,10.);
#4452=VECTOR('',#16157,10.);
#4453=VECTOR('',#16158,10.);
#4454=VECTOR('',#16159,10.);
#4455=VECTOR('',#16162,10.);
#4456=VECTOR('',#16163,10.);
#4457=VECTOR('',#16164,10.);
#4458=VECTOR('',#16169,10.);
#4459=VECTOR('',#16174,10.);
#4460=VECTOR('',#16175,10.);
#4461=VECTOR('',#16178,10.);
#4462=VECTOR('',#16179,10.);
#4463=VECTOR('',#16182,10.);
#4464=VECTOR('',#16183,10.);
#4465=VECTOR('',#16186,10.);
#4466=VECTOR('',#16187,10.);
#4467=VECTOR('',#16188,10.);
#4468=VECTOR('',#16193,10.);
#4469=VECTOR('',#16198,10.);
#4470=VECTOR('',#16199,10.);
#4471=VECTOR('',#16204,10.);
#4472=VECTOR('',#16207,10.);
#4473=VECTOR('',#16208,10.);
#4474=VECTOR('',#16213,10.);
#4475=VECTOR('',#16216,10.);
#4476=VECTOR('',#16219,10.);
#4477=VECTOR('',#16224,10.);
#4478=VECTOR('',#16225,10.);
#4479=VECTOR('',#16226,10.);
#4480=VECTOR('',#16229,10.);
#4481=VECTOR('',#16230,10.);
#4482=VECTOR('',#16231,10.);
#4483=VECTOR('',#16234,10.);
#4484=VECTOR('',#16235,10.);
#4485=VECTOR('',#16238,10.);
#4486=VECTOR('',#16239,10.);
#4487=VECTOR('',#16240,10.);
#4488=VECTOR('',#16243,10.);
#4489=VECTOR('',#16246,10.);
#4490=VECTOR('',#16247,10.);
#4491=VECTOR('',#16252,10.);
#4492=VECTOR('',#16255,10.);
#4493=VECTOR('',#16258,10.);
#4494=VECTOR('',#16259,10.);
#4495=VECTOR('',#16262,10.);
#4496=VECTOR('',#16263,10.);
#4497=VECTOR('',#16264,10.);
#4498=VECTOR('',#16269,10.);
#4499=VECTOR('',#16274,10.);
#4500=VECTOR('',#16275,10.);
#4501=VECTOR('',#16294,10.);
#4502=VECTOR('',#16297,2.25);
#4503=VECTOR('',#16304,2.25);
#4504=VECTOR('',#16309,10.);
#4505=VECTOR('',#16310,10.);
#4506=VECTOR('',#16321,10.);
#4507=VECTOR('',#16322,10.);
#4508=VECTOR('',#16323,10.);
#4509=VECTOR('',#16324,10.);
#4510=VECTOR('',#16329,10.);
#4511=VECTOR('',#16334,10.);
#4512=VECTOR('',#16335,10.);
#4513=VECTOR('',#16336,10.);
#4514=VECTOR('',#16341,10.);
#4515=VECTOR('',#16346,10.);
#4516=VECTOR('',#16347,10.);
#4517=VECTOR('',#16348,10.);
#4518=VECTOR('',#16351,10.);
#4519=VECTOR('',#16352,10.);
#4520=VECTOR('',#16355,10.);
#4521=VECTOR('',#16360,10.);
#4522=VECTOR('',#16361,10.);
#4523=VECTOR('',#16364,10.);
#4524=VECTOR('',#16365,10.);
#4525=VECTOR('',#16366,10.);
#4526=VECTOR('',#16367,10.);
#4527=VECTOR('',#16370,10.);
#4528=VECTOR('',#16371,10.);
#4529=VECTOR('',#16372,10.);
#4530=VECTOR('',#16373,10.);
#4531=VECTOR('',#16376,10.);
#4532=VECTOR('',#16377,10.);
#4533=VECTOR('',#16378,10.);
#4534=VECTOR('',#16381,10.);
#4535=VECTOR('',#16388,10.);
#4536=VECTOR('',#16389,10.);
#4537=VECTOR('',#16390,10.);
#4538=VECTOR('',#16391,10.);
#4539=VECTOR('',#16394,10.);
#4540=VECTOR('',#16401,10.);
#4541=VECTOR('',#16402,10.);
#4542=VECTOR('',#16403,10.);
#4543=VECTOR('',#16406,10.);
#4544=VECTOR('',#16413,10.);
#4545=VECTOR('',#16414,10.);
#4546=VECTOR('',#16419,10.);
#4547=VECTOR('',#16424,10.);
#4548=VECTOR('',#16425,10.);
#4549=VECTOR('',#16426,10.);
#4550=VECTOR('',#16427,10.);
#4551=VECTOR('',#16430,10.);
#4552=VECTOR('',#16433,10.);
#4553=VECTOR('',#16434,10.);
#4554=VECTOR('',#16435,10.);
#4555=VECTOR('',#16436,10.);
#4556=VECTOR('',#16437,10.);
#4557=VECTOR('',#16440,10.);
#4558=VECTOR('',#16441,10.);
#4559=VECTOR('',#16444,10.);
#4560=VECTOR('',#16445,10.);
#4561=VECTOR('',#16448,10.);
#4562=VECTOR('',#16451,10.);
#4563=VECTOR('',#16454,10.);
#4564=VECTOR('',#16457,10.);
#4565=VECTOR('',#16460,10.);
#4566=VECTOR('',#16461,10.);
#4567=VECTOR('',#16464,10.);
#4568=VECTOR('',#16465,10.);
#4569=VECTOR('',#16466,10.);
#4570=VECTOR('',#16467,10.);
#4571=VECTOR('',#16468,10.);
#4572=VECTOR('',#16473,10.);
#4573=VECTOR('',#16474,10.);
#4574=VECTOR('',#16475,10.);
#4575=VECTOR('',#16478,10.);
#4576=VECTOR('',#16479,10.);
#4577=VECTOR('',#16482,10.);
#4578=VECTOR('',#16483,10.);
#4579=VECTOR('',#16484,10.);
#4580=VECTOR('',#16487,10.);
#4581=VECTOR('',#16488,10.);
#4582=VECTOR('',#16489,10.);
#4583=VECTOR('',#16492,10.);
#4584=VECTOR('',#16493,10.);
#4585=VECTOR('',#16494,10.);
#4586=VECTOR('',#16495,10.);
#4587=VECTOR('',#16498,10.);
#4588=VECTOR('',#16499,10.);
#4589=VECTOR('',#16504,10.);
#4590=VECTOR('',#16507,10.);
#4591=VECTOR('',#16508,10.);
#4592=VECTOR('',#16511,10.);
#4593=VECTOR('',#16512,10.);
#4594=VECTOR('',#16515,10.);
#4595=VECTOR('',#16518,10.);
#4596=VECTOR('',#16521,10.);
#4597=VECTOR('',#16524,10.);
#4598=VECTOR('',#16525,10.);
#4599=VECTOR('',#16528,10.);
#4600=VECTOR('',#16529,10.);
#4601=VECTOR('',#16532,10.);
#4602=VECTOR('',#16537,10.);
#4603=VECTOR('',#16540,10.);
#4604=VECTOR('',#16543,10.);
#4605=VECTOR('',#16544,10.);
#4606=VECTOR('',#16547,10.);
#4607=VECTOR('',#16548,10.);
#4608=VECTOR('',#16551,10.);
#4609=VECTOR('',#16558,10.);
#4610=VECTOR('',#16559,10.);
#4611=VECTOR('',#16560,10.);
#4612=VECTOR('',#16563,10.);
#4613=VECTOR('',#16570,10.);
#4614=VECTOR('',#16573,10.);
#4615=VECTOR('',#16582,10.);
#4616=VECTOR('',#16583,10.);
#4617=VECTOR('',#16584,10.);
#4618=VECTOR('',#16589,10.);
#4619=VECTOR('',#16596,10.);
#4620=VECTOR('',#16597,10.);
#4621=VECTOR('',#16598,10.);
#4622=VECTOR('',#16601,10.);
#4623=VECTOR('',#16608,10.);
#4624=VECTOR('',#16617,10.);
#4625=VECTOR('',#16618,10.);
#4626=VECTOR('',#16619,10.);
#4627=VECTOR('',#16622,10.);
#4628=VECTOR('',#16623,10.);
#4629=VECTOR('',#16630,10.);
#4630=VECTOR('',#16637,10.);
#4631=VECTOR('',#16638,10.);
#4632=VECTOR('',#16641,10.);
#4633=VECTOR('',#16646,10.);
#4634=VECTOR('',#16649,10.);
#4635=VECTOR('',#16652,10.);
#4636=VECTOR('',#16663,10.);
#4637=VECTOR('',#16664,10.);
#4638=VECTOR('',#16667,10.);
#4639=VECTOR('',#16668,10.);
#4640=VECTOR('',#16671,10.);
#4641=VECTOR('',#16672,10.);
#4642=VECTOR('',#16675,10.);
#4643=VECTOR('',#16676,10.);
#4644=VECTOR('',#16679,10.);
#4645=VECTOR('',#16680,10.);
#4646=VECTOR('',#16693,10.);
#4647=VECTOR('',#16694,10.);
#4648=VECTOR('',#16695,10.);
#4649=VECTOR('',#16714,10.);
#4650=VECTOR('',#16719,2.25);
#4651=VECTOR('',#16722,2.25);
#4652=VECTOR('',#16729,2.15);
#4653=VECTOR('',#16732,2.15);
#4654=VECTOR('',#16735,10.);
#4655=VECTOR('',#16738,10.);
#4656=VECTOR('',#16741,10.);
#4657=VECTOR('',#16744,10.);
#4658=VECTOR('',#16753,10.);
#4659=VECTOR('',#16754,10.);
#4660=VECTOR('',#16755,10.);
#4661=VECTOR('',#16756,10.);
#4662=VECTOR('',#16759,10.);
#4663=VECTOR('',#16766,10.);
#4664=VECTOR('',#16767,10.);
#4665=VECTOR('',#16768,10.);
#4666=VECTOR('',#16771,10.);
#4667=VECTOR('',#16772,10.);
#4668=VECTOR('',#16773,10.);
#4669=VECTOR('',#16776,10.);
#4670=VECTOR('',#16781,10.);
#4671=VECTOR('',#16782,10.);
#4672=VECTOR('',#16785,10.);
#4673=VECTOR('',#16786,10.);
#4674=VECTOR('',#16787,10.);
#4675=VECTOR('',#16790,10.);
#4676=VECTOR('',#16795,10.);
#4677=VECTOR('',#16796,10.);
#4678=VECTOR('',#16799,10.);
#4679=VECTOR('',#16800,10.);
#4680=VECTOR('',#16801,10.);
#4681=VECTOR('',#16802,10.);
#4682=VECTOR('',#16803,10.);
#4683=VECTOR('',#16804,10.);
#4684=VECTOR('',#16805,10.);
#4685=VECTOR('',#16808,10.);
#4686=VECTOR('',#16809,10.);
#4687=VECTOR('',#16810,10.);
#4688=VECTOR('',#16811,10.);
#4689=VECTOR('',#16814,10.);
#4690=VECTOR('',#16821,10.);
#4691=VECTOR('',#16822,10.);
#4692=VECTOR('',#16823,10.);
#4693=VECTOR('',#16826,10.);
#4694=VECTOR('',#16827,10.);
#4695=VECTOR('',#16828,10.);
#4696=VECTOR('',#16831,10.);
#4697=VECTOR('',#16836,10.);
#4698=VECTOR('',#16837,10.);
#4699=VECTOR('',#16840,10.);
#4700=VECTOR('',#16841,10.);
#4701=VECTOR('',#16842,10.);
#4702=VECTOR('',#16845,10.);
#4703=VECTOR('',#16846,10.);
#4704=VECTOR('',#16847,10.);
#4705=VECTOR('',#16850,10.);
#4706=VECTOR('',#16851,10.);
#4707=VECTOR('',#16852,10.);
#4708=VECTOR('',#16853,10.);
#4709=VECTOR('',#16856,10.);
#4710=VECTOR('',#16857,10.);
#4711=VECTOR('',#16858,10.);
#4712=VECTOR('',#16859,10.);
#4713=VECTOR('',#16862,10.);
#4714=VECTOR('',#16863,10.);
#4715=VECTOR('',#16866,10.);
#4716=VECTOR('',#16867,10.);
#4717=VECTOR('',#16870,10.);
#4718=VECTOR('',#16871,10.);
#4719=VECTOR('',#16872,10.);
#4720=VECTOR('',#16877,2.4);
#4721=VECTOR('',#16882,2.15);
#4722=VECTOR('',#16887,10.);
#4723=VECTOR('',#16892,2.4);
#4724=VECTOR('',#16897,2.15);
#4725=VECTOR('',#16902,10.);
#4726=VECTOR('',#16905,2.4);
#4727=VECTOR('',#16910,10.);
#4728=VECTOR('',#16911,10.);
#4729=VECTOR('',#16912,10.);
#4730=VECTOR('',#16913,10.);
#4731=VECTOR('',#16914,10.);
#4732=VECTOR('',#16915,10.);
#4733=VECTOR('',#16918,10.);
#4734=VECTOR('',#16919,10.);
#4735=VECTOR('',#16920,10.);
#4736=VECTOR('',#16923,10.);
#4737=VECTOR('',#16924,10.);
#4738=VECTOR('',#16927,10.);
#4739=VECTOR('',#16928,10.);
#4740=VECTOR('',#16929,10.);
#4741=VECTOR('',#16932,10.);
#4742=VECTOR('',#16933,10.);
#4743=VECTOR('',#16936,10.);
#4744=VECTOR('',#16939,10.);
#4745=VECTOR('',#16942,10.);
#4746=VECTOR('',#16943,10.);
#4747=VECTOR('',#16946,10.);
#4748=VECTOR('',#16949,10.);
#4749=VECTOR('',#16952,2.4);
#4750=VECTOR('',#16957,10.);
#4751=VECTOR('',#16958,10.);
#4752=VECTOR('',#16959,10.);
#4753=VECTOR('',#16960,10.);
#4754=VECTOR('',#16961,10.);
#4755=VECTOR('',#16962,10.);
#4756=VECTOR('',#16965,10.);
#4757=VECTOR('',#16966,10.);
#4758=VECTOR('',#16967,10.);
#4759=VECTOR('',#16970,10.);
#4760=VECTOR('',#16975,10.);
#4761=VECTOR('',#16976,10.);
#4762=VECTOR('',#16979,10.);
#4763=VECTOR('',#16980,10.);
#4764=VECTOR('',#16981,10.);
#4765=VECTOR('',#16982,10.);
#4766=VECTOR('',#16985,10.);
#4767=VECTOR('',#16986,10.);
#4768=VECTOR('',#16987,10.);
#4769=VECTOR('',#16990,10.);
#4770=VECTOR('',#16991,10.);
#4771=VECTOR('',#16992,10.);
#4772=VECTOR('',#16993,10.);
#4773=VECTOR('',#16996,10.);
#4774=VECTOR('',#16997,10.);
#4775=VECTOR('',#16998,10.);
#4776=VECTOR('',#17001,10.);
#4777=VECTOR('',#17002,10.);
#4778=VECTOR('',#17005,10.);
#4779=VECTOR('',#17006,10.);
#4780=VECTOR('',#17009,10.);
#4781=VECTOR('',#17010,10.);
#4782=VECTOR('',#17013,10.);
#4783=VECTOR('',#17016,10.);
#4784=VECTOR('',#17019,10.);
#4785=VECTOR('',#17022,10.);
#4786=VECTOR('',#17023,10.);
#4787=VECTOR('',#17024,10.);
#4788=VECTOR('',#17027,10.);
#4789=VECTOR('',#17028,10.);
#4790=VECTOR('',#17029,10.);
#4791=VECTOR('',#17032,10.);
#4792=VECTOR('',#17033,10.);
#4793=VECTOR('',#17034,10.);
#4794=VECTOR('',#17037,10.);
#4795=VECTOR('',#17038,10.);
#4796=VECTOR('',#17039,10.);
#4797=VECTOR('',#17042,10.);
#4798=VECTOR('',#17043,10.);
#4799=VECTOR('',#17044,10.);
#4800=VECTOR('',#17045,10.);
#4801=VECTOR('',#17048,10.);
#4802=VECTOR('',#17049,10.);
#4803=VECTOR('',#17052,10.);
#4804=VECTOR('',#17053,10.);
#4805=VECTOR('',#17054,10.);
#4806=VECTOR('',#17055,10.);
#4807=VECTOR('',#17058,10.);
#4808=VECTOR('',#17061,10.);
#4809=VECTOR('',#17062,10.);
#4810=VECTOR('',#17065,10.);
#4811=VECTOR('',#17066,10.);
#4812=VECTOR('',#17067,10.);
#4813=VECTOR('',#17070,10.);
#4814=VECTOR('',#17071,10.);
#4815=VECTOR('',#17072,10.);
#4816=VECTOR('',#17075,10.);
#4817=VECTOR('',#17076,10.);
#4818=VECTOR('',#17077,10.);
#4819=VECTOR('',#17080,10.);
#4820=VECTOR('',#17081,10.);
#4821=VECTOR('',#17082,10.);
#4822=VECTOR('',#17085,10.);
#4823=VECTOR('',#17086,10.);
#4824=VECTOR('',#17087,10.);
#4825=VECTOR('',#17090,10.);
#4826=VECTOR('',#17091,10.);
#4827=VECTOR('',#17092,10.);
#4828=VECTOR('',#17093,10.);
#4829=VECTOR('',#17096,10.);
#4830=VECTOR('',#17097,10.);
#4831=VECTOR('',#17100,10.);
#4832=VECTOR('',#17101,10.);
#4833=VECTOR('',#17102,10.);
#4834=VECTOR('',#17103,10.);
#4835=VECTOR('',#17106,10.);
#4836=VECTOR('',#17109,10.);
#4837=VECTOR('',#17110,10.);
#4838=VECTOR('',#17113,10.);
#4839=VECTOR('',#17114,10.);
#4840=VECTOR('',#17115,10.);
#4841=VECTOR('',#17118,10.);
#4842=VECTOR('',#17119,10.);
#4843=VECTOR('',#17120,10.);
#4844=VECTOR('',#17121,10.);
#4845=VECTOR('',#17124,10.);
#4846=VECTOR('',#17125,10.);
#4847=VECTOR('',#17128,10.);
#4848=VECTOR('',#17129,10.);
#4849=VECTOR('',#17130,10.);
#4850=VECTOR('',#17133,10.);
#4851=VECTOR('',#17134,10.);
#4852=VECTOR('',#17135,10.);
#4853=VECTOR('',#17136,10.);
#4854=VECTOR('',#17139,10.);
#4855=VECTOR('',#17140,10.);
#4856=VECTOR('',#17141,10.);
#4857=VECTOR('',#17144,10.);
#4858=VECTOR('',#17145,10.);
#4859=VECTOR('',#17146,10.);
#4860=VECTOR('',#17149,10.);
#4861=VECTOR('',#17150,10.);
#4862=VECTOR('',#17153,10.);
#4863=VECTOR('',#17154,10.);
#4864=VECTOR('',#17155,10.);
#4865=VECTOR('',#17158,10.);
#4866=VECTOR('',#17159,10.);
#4867=VECTOR('',#17162,10.);
#4868=VECTOR('',#17163,10.);
#4869=VECTOR('',#17166,10.);
#4870=VECTOR('',#17167,10.);
#4871=VECTOR('',#17168,10.);
#4872=VECTOR('',#17169,10.);
#4873=VECTOR('',#17170,10.);
#4874=VECTOR('',#17171,10.);
#4875=VECTOR('',#17172,10.);
#4876=VECTOR('',#17173,10.);
#4877=VECTOR('',#17174,10.);
#4878=VECTOR('',#17175,10.);
#4879=VECTOR('',#17176,10.);
#4880=VECTOR('',#17177,10.);
#4881=VECTOR('',#17180,10.);
#4882=VECTOR('',#17183,10.);
#4883=VECTOR('',#17184,10.);
#4884=VECTOR('',#17185,10.);
#4885=VECTOR('',#17188,10.);
#4886=VECTOR('',#17195,10.);
#4887=VECTOR('',#17196,10.);
#4888=VECTOR('',#17197,10.);
#4889=VECTOR('',#17200,10.);
#4890=VECTOR('',#17207,10.);
#4891=VECTOR('',#17208,10.);
#4892=VECTOR('',#17209,10.);
#4893=VECTOR('',#17212,10.);
#4894=VECTOR('',#17219,10.);
#4895=VECTOR('',#17220,10.);
#4896=VECTOR('',#17221,10.);
#4897=VECTOR('',#17230,10.);
#4898=VECTOR('',#17233,10.);
#4899=VECTOR('',#17236,10.);
#4900=VECTOR('',#17237,10.);
#4901=VECTOR('',#17248,10.);
#4902=VECTOR('',#17249,10.);
#4903=VECTOR('',#17252,10.);
#4904=VECTOR('',#17253,10.);
#4905=VECTOR('',#17256,10.);
#4906=VECTOR('',#17257,10.);
#4907=VECTOR('',#17260,10.);
#4908=VECTOR('',#17261,10.);
#4909=VECTOR('',#17266,10.);
#4910=VECTOR('',#17271,10.);
#4911=VECTOR('',#17272,10.);
#4912=VECTOR('',#17273,10.);
#4913=VECTOR('',#17278,10.);
#4914=VECTOR('',#17283,10.);
#4915=VECTOR('',#17284,10.);
#4916=VECTOR('',#17285,10.);
#4917=VECTOR('',#17288,10.);
#4918=VECTOR('',#17293,10.);
#4919=VECTOR('',#17294,10.);
#4920=VECTOR('',#17297,10.);
#4921=VECTOR('',#17302,10.);
#4922=VECTOR('',#17303,10.);
#4923=VECTOR('',#17306,10.);
#4924=VECTOR('',#17309,10.);
#4925=VECTOR('',#17312,10.);
#4926=VECTOR('',#17315,10.);
#4927=VECTOR('',#17316,10.);
#4928=VECTOR('',#17319,10.);
#4929=VECTOR('',#17322,10.);
#4930=VECTOR('',#17325,10.);
#4931=VECTOR('',#17328,10.);
#4932=VECTOR('',#17333,10.);
#4933=VECTOR('',#17338,10.);
#4934=VECTOR('',#17343,10.);
#4935=VECTOR('',#17344,10.);
#4936=VECTOR('',#17347,10.);
#4937=VECTOR('',#17352,10.);
#4938=VECTOR('',#17355,1.3);
#4939=VECTOR('',#17358,10.);
#4940=VECTOR('',#17359,10.);
#4941=VECTOR('',#17362,10.);
#4942=VECTOR('',#17365,10.);
#4943=VECTOR('',#17368,1.3);
#4944=VECTOR('',#17373,2.75);
#4945=VECTOR('',#17378,2.5);
#4946=VECTOR('',#17385,2.75);
#4947=VECTOR('',#17388,10.);
#4948=VECTOR('',#17389,10.);
#4949=VECTOR('',#17396,10.);
#4950=VECTOR('',#17399,10.);
#4951=VECTOR('',#17404,10.);
#4952=VECTOR('',#17407,10.);
#4953=VECTOR('',#17412,10.);
#4954=VECTOR('',#17423,4.3);
#4955=VECTOR('',#17430,4.2);
#4956=VECTOR('',#17433,10.);
#4957=VECTOR('',#17436,10.);
#4958=VECTOR('',#17439,10.);
#4959=VECTOR('',#17442,10.);
#4960=VECTOR('',#17453,4.3);
#4961=VECTOR('',#17456,10.);
#4962=VECTOR('',#17459,10.);
#4963=VECTOR('',#17462,10.);
#4964=VECTOR('',#17465,10.);
#4965=VECTOR('',#17474,10.);
#4966=VECTOR('',#17475,10.);
#4967=VECTOR('',#17476,10.);
#4968=VECTOR('',#17481,10.);
#4969=VECTOR('',#17484,10.);
#4970=VECTOR('',#17485,10.);
#4971=VECTOR('',#17490,10.);
#4972=VECTOR('',#17493,10.);
#4973=VECTOR('',#17494,10.);
#4974=VECTOR('',#17499,10.);
#4975=VECTOR('',#17502,10.);
#4976=VECTOR('',#17503,10.);
#4977=VECTOR('',#17510,10.);
#4978=VECTOR('',#17513,10.);
#4979=VECTOR('',#17516,10.);
#4980=VECTOR('',#17517,10.);
#4981=VECTOR('',#17520,10.);
#4982=VECTOR('',#17525,10.);
#4983=VECTOR('',#17526,10.);
#4984=VECTOR('',#17529,10.);
#4985=VECTOR('',#17530,10.);
#4986=VECTOR('',#17531,10.);
#4987=VECTOR('',#17532,10.);
#4988=VECTOR('',#17535,10.);
#4989=VECTOR('',#17540,10.);
#4990=VECTOR('',#17541,10.);
#4991=VECTOR('',#17544,10.);
#4992=VECTOR('',#17549,10.);
#4993=VECTOR('',#17550,10.);
#4994=VECTOR('',#17553,10.);
#4995=VECTOR('',#17560,10.);
#4996=VECTOR('',#17561,10.);
#4997=VECTOR('',#17562,10.);
#4998=VECTOR('',#17571,10.);
#4999=VECTOR('',#17574,10.);
#5000=VECTOR('',#17577,10.);
#5001=VECTOR('',#17578,10.);
#5002=VECTOR('',#17581,10.);
#5003=VECTOR('',#17586,10.);
#5004=VECTOR('',#17587,10.);
#5005=VECTOR('',#17590,10.);
#5006=VECTOR('',#17593,10.);
#5007=VECTOR('',#17594,10.);
#5008=VECTOR('',#17597,10.);
#5009=VECTOR('',#17600,10.);
#5010=VECTOR('',#17603,10.);
#5011=VECTOR('',#17606,10.);
#5012=VECTOR('',#17607,10.);
#5013=VECTOR('',#17610,10.);
#5014=VECTOR('',#17615,10.);
#5015=VECTOR('',#17616,10.);
#5016=VECTOR('',#17623,10.);
#5017=VECTOR('',#17624,10.);
#5018=VECTOR('',#17627,10.);
#5019=VECTOR('',#17634,1.45);
#5020=VECTOR('',#17637,1.45);
#5021=VECTOR('',#17640,10.);
#5022=VECTOR('',#17643,10.);
#5023=VECTOR('',#17650,10.);
#5024=VECTOR('',#17651,10.);
#5025=VECTOR('',#17652,10.);
#5026=VECTOR('',#17653,10.);
#5027=VECTOR('',#17656,10.);
#5028=VECTOR('',#17657,10.);
#5029=VECTOR('',#17658,10.);
#5030=VECTOR('',#17661,10.);
#5031=VECTOR('',#17662,10.);
#5032=VECTOR('',#17663,10.);
#5033=VECTOR('',#17666,10.);
#5034=VECTOR('',#17667,10.);
#5035=VECTOR('',#17672,10.);
#5036=VECTOR('',#17673,10.);
#5037=VECTOR('',#17674,10.);
#5038=VECTOR('',#17675,10.);
#5039=VECTOR('',#17678,10.);
#5040=VECTOR('',#17679,10.);
#5041=VECTOR('',#17680,10.);
#5042=VECTOR('',#17683,10.);
#5043=VECTOR('',#17684,10.);
#5044=VECTOR('',#17685,10.);
#5045=VECTOR('',#17688,10.);
#5046=VECTOR('',#17689,10.);
#5047=VECTOR('',#17694,10.);
#5048=VECTOR('',#17695,10.);
#5049=VECTOR('',#17696,10.);
#5050=VECTOR('',#17697,10.);
#5051=VECTOR('',#17700,10.);
#5052=VECTOR('',#17701,10.);
#5053=VECTOR('',#17702,10.);
#5054=VECTOR('',#17705,10.);
#5055=VECTOR('',#17706,10.);
#5056=VECTOR('',#17707,10.);
#5057=VECTOR('',#17710,10.);
#5058=VECTOR('',#17711,10.);
#5059=VECTOR('',#17716,10.);
#5060=VECTOR('',#17717,10.);
#5061=VECTOR('',#17718,10.);
#5062=VECTOR('',#17719,10.);
#5063=VECTOR('',#17722,10.);
#5064=VECTOR('',#17723,10.);
#5065=VECTOR('',#17724,10.);
#5066=VECTOR('',#17727,10.);
#5067=VECTOR('',#17728,10.);
#5068=VECTOR('',#17729,10.);
#5069=VECTOR('',#17732,10.);
#5070=VECTOR('',#17733,10.);
#5071=VECTOR('',#17742,10.);
#5072=VECTOR('',#17743,10.);
#5073=VECTOR('',#17744,10.);
#5074=VECTOR('',#17747,10.);
#5075=VECTOR('',#17748,10.);
#5076=VECTOR('',#17749,10.);
#5077=VECTOR('',#17752,10.);
#5078=VECTOR('',#17753,10.);
#5079=VECTOR('',#17754,10.);
#5080=VECTOR('',#17757,10.);
#5081=VECTOR('',#17758,10.);
#5082=VECTOR('',#17759,10.);
#5083=VECTOR('',#17762,10.);
#5084=VECTOR('',#17763,10.);
#5085=VECTOR('',#17764,10.);
#5086=VECTOR('',#17767,10.);
#5087=VECTOR('',#17768,10.);
#5088=VECTOR('',#17769,10.);
#5089=VECTOR('',#17772,10.);
#5090=VECTOR('',#17773,10.);
#5091=VECTOR('',#17774,10.);
#5092=VECTOR('',#17777,10.);
#5093=VECTOR('',#17778,10.);
#5094=VECTOR('',#17781,10.);
#5095=VECTOR('',#17782,10.);
#5096=VECTOR('',#17783,10.);
#5097=VECTOR('',#17786,10.);
#5098=VECTOR('',#17787,10.);
#5099=VECTOR('',#17790,10.);
#5100=VECTOR('',#17791,10.);
#5101=VECTOR('',#17794,10.);
#5102=VECTOR('',#17795,10.);
#5103=VECTOR('',#17798,10.);
#5104=VECTOR('',#17799,10.);
#5105=VECTOR('',#17802,10.);
#5106=VECTOR('',#17803,10.);
#5107=VECTOR('',#17806,10.);
#5108=VECTOR('',#17807,10.);
#5109=VECTOR('',#17810,10.);
#5110=VECTOR('',#17811,10.);
#5111=VECTOR('',#17814,10.);
#5112=VECTOR('',#17815,10.);
#5113=VECTOR('',#17818,10.);
#5114=VECTOR('',#17819,10.);
#5115=VECTOR('',#17822,10.);
#5116=VECTOR('',#17823,10.);
#5117=VECTOR('',#17826,10.);
#5118=VECTOR('',#17827,10.);
#5119=VECTOR('',#17846,4.05);
#5120=VECTOR('',#17851,4.);
#5121=VECTOR('',#17856,4.);
#5122=VECTOR('',#17859,4.);
#5123=VECTOR('',#17862,4.);
#5124=VECTOR('',#17865,4.);
#5125=VECTOR('',#17868,4.);
#5126=VECTOR('',#17871,4.);
#5127=VECTOR('',#17874,4.);
#5128=VECTOR('',#17877,4.);
#5129=VECTOR('',#17880,4.);
#5130=VECTOR('',#17883,4.);
#5131=VECTOR('',#17886,4.);
#5132=VECTOR('',#17889,4.);
#5133=VECTOR('',#17892,4.);
#5134=VECTOR('',#17895,4.);
#5135=VECTOR('',#17898,4.);
#5136=VECTOR('',#17901,4.);
#5137=VECTOR('',#17904,4.);
#5138=VECTOR('',#17907,4.);
#5139=VECTOR('',#17910,4.);
#5140=VECTOR('',#17913,4.);
#5141=VECTOR('',#17916,4.);
#5142=VECTOR('',#17919,4.);
#5143=VECTOR('',#17922,4.);
#5144=VECTOR('',#17925,4.);
#5145=VECTOR('',#17928,4.);
#5146=VECTOR('',#17931,4.);
#5147=VECTOR('',#17934,4.);
#5148=VECTOR('',#17937,3.52375);
#5149=VECTOR('',#17942,3.52375);
#5150=VECTOR('',#17945,3.52375);
#5151=VECTOR('',#17948,3.52375);
#5152=VECTOR('',#17951,3.52375);
#5153=VECTOR('',#17954,3.52375);
#5154=VECTOR('',#17957,3.52375);
#5155=VECTOR('',#17960,3.52375);
#5156=VECTOR('',#17963,3.52375);
#5157=VECTOR('',#17966,3.52375);
#5158=VECTOR('',#17969,3.52375);
#5159=VECTOR('',#17972,3.52375);
#5160=VECTOR('',#17975,3.52375);
#5161=VECTOR('',#17978,3.52375);
#5162=VECTOR('',#17981,3.52375);
#5163=VECTOR('',#17984,3.52375);
#5164=VECTOR('',#17987,3.52375);
#5165=VECTOR('',#17990,3.52375);
#5166=VECTOR('',#17993,3.52375);
#5167=VECTOR('',#17996,3.52375);
#5168=VECTOR('',#17999,3.52375);
#5169=VECTOR('',#18002,3.52375);
#5170=VECTOR('',#18005,3.52375);
#5171=VECTOR('',#18008,3.52375);
#5172=VECTOR('',#18011,3.52375);
#5173=VECTOR('',#18014,3.52375);
#5174=VECTOR('',#18017,3.52375);
#5175=VECTOR('',#18022,4.8);
#5176=VECTOR('',#18125,5.);
#5177=VECTOR('',#18128,10.);
#5178=VECTOR('',#18129,10.);
#5179=VECTOR('',#18132,10.);
#5180=VECTOR('',#18133,10.);
#5181=VECTOR('',#18136,10.);
#5182=VECTOR('',#18137,10.);
#5183=VECTOR('',#18140,10.);
#5184=VECTOR('',#18141,10.);
#5185=VECTOR('',#18144,10.);
#5186=VECTOR('',#18145,10.);
#5187=VECTOR('',#18148,10.);
#5188=VECTOR('',#18149,10.);
#5189=VECTOR('',#18152,10.);
#5190=VECTOR('',#18153,10.);
#5191=VECTOR('',#18156,10.);
#5192=VECTOR('',#18157,10.);
#5193=VECTOR('',#18160,10.);
#5194=VECTOR('',#18161,10.);
#5195=VECTOR('',#18164,10.);
#5196=VECTOR('',#18165,10.);
#5197=VECTOR('',#18168,10.);
#5198=VECTOR('',#18169,10.);
#5199=VECTOR('',#18172,10.);
#5200=VECTOR('',#18173,10.);
#5201=VECTOR('',#18176,10.);
#5202=VECTOR('',#18177,10.);
#5203=VECTOR('',#18180,10.);
#5204=VECTOR('',#18181,10.);
#5205=VECTOR('',#18184,10.);
#5206=VECTOR('',#18185,10.);
#5207=VECTOR('',#18188,10.);
#5208=VECTOR('',#18189,10.);
#5209=VECTOR('',#18192,10.);
#5210=VECTOR('',#18193,10.);
#5211=VECTOR('',#18196,10.);
#5212=VECTOR('',#18197,10.);
#5213=VECTOR('',#18200,10.);
#5214=VECTOR('',#18201,10.);
#5215=VECTOR('',#18204,10.);
#5216=VECTOR('',#18205,10.);
#5217=VECTOR('',#18208,10.);
#5218=VECTOR('',#18209,10.);
#5219=VECTOR('',#18212,10.);
#5220=VECTOR('',#18213,10.);
#5221=VECTOR('',#18216,10.);
#5222=VECTOR('',#18217,10.);
#5223=VECTOR('',#18220,10.);
#5224=VECTOR('',#18221,10.);
#5225=VECTOR('',#18240,10.);
#5226=VECTOR('',#18241,10.);
#5227=VECTOR('',#18242,10.);
#5228=VECTOR('',#18245,10.);
#5229=VECTOR('',#18248,10.);
#5230=VECTOR('',#18253,10.);
#5231=VECTOR('',#18254,10.);
#5232=VECTOR('',#18255,10.);
#5233=VECTOR('',#18258,10.);
#5234=VECTOR('',#18261,10.);
#5235=VECTOR('',#18266,10.);
#5236=VECTOR('',#18267,10.);
#5237=VECTOR('',#18268,10.);
#5238=VECTOR('',#18271,10.);
#5239=VECTOR('',#18274,10.);
#5240=VECTOR('',#18279,10.);
#5241=VECTOR('',#18280,10.);
#5242=VECTOR('',#18281,10.);
#5243=VECTOR('',#18284,10.);
#5244=VECTOR('',#18287,10.);
#5245=VECTOR('',#18292,10.);
#5246=VECTOR('',#18293,10.);
#5247=VECTOR('',#18294,10.);
#5248=VECTOR('',#18297,10.);
#5249=VECTOR('',#18300,10.);
#5250=VECTOR('',#18305,10.);
#5251=VECTOR('',#18306,10.);
#5252=VECTOR('',#18307,10.);
#5253=VECTOR('',#18310,10.);
#5254=VECTOR('',#18313,10.);
#5255=VECTOR('',#18318,10.);
#5256=VECTOR('',#18319,10.);
#5257=VECTOR('',#18320,10.);
#5258=VECTOR('',#18323,10.);
#5259=VECTOR('',#18326,10.);
#5260=VECTOR('',#18331,10.);
#5261=VECTOR('',#18332,10.);
#5262=VECTOR('',#18333,10.);
#5263=VECTOR('',#18336,10.);
#5264=VECTOR('',#18339,10.);
#5265=VECTOR('',#18344,10.);
#5266=VECTOR('',#18345,10.);
#5267=VECTOR('',#18346,10.);
#5268=VECTOR('',#18349,10.);
#5269=VECTOR('',#18352,10.);
#5270=VECTOR('',#18357,10.);
#5271=VECTOR('',#18358,10.);
#5272=VECTOR('',#18359,10.);
#5273=VECTOR('',#18362,10.);
#5274=VECTOR('',#18365,10.);
#5275=VECTOR('',#18370,10.);
#5276=VECTOR('',#18371,10.);
#5277=VECTOR('',#18372,10.);
#5278=VECTOR('',#18375,10.);
#5279=VECTOR('',#18378,10.);
#5280=VECTOR('',#18383,10.);
#5281=VECTOR('',#18384,10.);
#5282=VECTOR('',#18385,10.);
#5283=VECTOR('',#18388,10.);
#5284=VECTOR('',#18391,10.);
#5285=VECTOR('',#18396,10.);
#5286=VECTOR('',#18397,10.);
#5287=VECTOR('',#18398,10.);
#5288=VECTOR('',#18401,10.);
#5289=VECTOR('',#18404,10.);
#5290=VECTOR('',#18409,10.);
#5291=VECTOR('',#18410,10.);
#5292=VECTOR('',#18411,10.);
#5293=VECTOR('',#18414,10.);
#5294=VECTOR('',#18417,10.);
#5295=VECTOR('',#18422,10.);
#5296=VECTOR('',#18423,10.);
#5297=VECTOR('',#18424,10.);
#5298=VECTOR('',#18427,10.);
#5299=VECTOR('',#18430,10.);
#5300=VECTOR('',#18435,10.);
#5301=VECTOR('',#18436,10.);
#5302=VECTOR('',#18437,10.);
#5303=VECTOR('',#18440,10.);
#5304=VECTOR('',#18443,10.);
#5305=VECTOR('',#18448,10.);
#5306=VECTOR('',#18449,10.);
#5307=VECTOR('',#18450,10.);
#5308=VECTOR('',#18453,10.);
#5309=VECTOR('',#18456,10.);
#5310=VECTOR('',#18461,10.);
#5311=VECTOR('',#18462,10.);
#5312=VECTOR('',#18463,10.);
#5313=VECTOR('',#18466,10.);
#5314=VECTOR('',#18469,10.);
#5315=VECTOR('',#18474,10.);
#5316=VECTOR('',#18475,10.);
#5317=VECTOR('',#18476,10.);
#5318=VECTOR('',#18479,10.);
#5319=VECTOR('',#18482,10.);
#5320=VECTOR('',#18487,10.);
#5321=VECTOR('',#18488,10.);
#5322=VECTOR('',#18489,10.);
#5323=VECTOR('',#18492,10.);
#5324=VECTOR('',#18495,10.);
#5325=VECTOR('',#18500,10.);
#5326=VECTOR('',#18501,10.);
#5327=VECTOR('',#18502,10.);
#5328=VECTOR('',#18505,10.);
#5329=VECTOR('',#18508,10.);
#5330=VECTOR('',#18513,10.);
#5331=VECTOR('',#18514,10.);
#5332=VECTOR('',#18515,10.);
#5333=VECTOR('',#18518,10.);
#5334=VECTOR('',#18521,10.);
#5335=VECTOR('',#18526,10.);
#5336=VECTOR('',#18527,10.);
#5337=VECTOR('',#18528,10.);
#5338=VECTOR('',#18531,10.);
#5339=VECTOR('',#18534,10.);
#5340=VECTOR('',#18539,10.);
#5341=VECTOR('',#18540,10.);
#5342=VECTOR('',#18541,10.);
#5343=VECTOR('',#18544,10.);
#5344=VECTOR('',#18547,10.);
#5345=VECTOR('',#18556,3.8);
#5346=VECTOR('',#18563,4.75);
#5347=VECTOR('',#18570,3.);
#5348=VECTOR('',#18583,2.31);
#5349=VECTOR('',#18588,2.15);
#5350=VECTOR('',#18597,10.);
#5351=VECTOR('',#18598,10.);
#5352=VECTOR('',#18599,10.);
#5353=VECTOR('',#18606,10.);
#5354=VECTOR('',#18609,10.);
#5355=VECTOR('',#18612,10.);
#5356=VECTOR('',#18615,10.);
#5357=VECTOR('',#18618,10.);
#5358=VECTOR('',#18621,10.);
#5359=VECTOR('',#18624,10.);
#5360=VECTOR('',#18627,10.);
#5361=VECTOR('',#18630,10.);
#5362=VECTOR('',#18633,10.);
#5363=VECTOR('',#18636,10.);
#5364=VECTOR('',#18639,10.);
#5365=VECTOR('',#18642,10.);
#5366=VECTOR('',#18645,10.);
#5367=VECTOR('',#18648,10.);
#5368=VECTOR('',#18651,6.5);
#5369=VECTOR('',#18656,10.);
#5370=VECTOR('',#18659,10.);
#5371=VECTOR('',#18662,10.);
#5372=VECTOR('',#18665,10.);
#5373=VECTOR('',#18668,10.);
#5374=VECTOR('',#18671,10.);
#5375=VECTOR('',#18674,10.);
#5376=VECTOR('',#18677,10.);
#5377=VECTOR('',#18680,10.);
#5378=VECTOR('',#18683,10.);
#5379=VECTOR('',#18686,10.);
#5380=VECTOR('',#18689,10.);
#5381=VECTOR('',#18692,10.);
#5382=VECTOR('',#18695,10.);
#5383=VECTOR('',#18698,10.);
#5384=VECTOR('',#18701,10.);
#5385=VECTOR('',#18704,6.2);
#5386=VECTOR('',#18707,10.);
#5387=VECTOR('',#18708,10.);
#5388=VECTOR('',#18711,10.);
#5389=VECTOR('',#18712,10.);
#5390=VECTOR('',#18715,10.);
#5391=VECTOR('',#18716,10.);
#5392=VECTOR('',#18719,10.);
#5393=VECTOR('',#18720,10.);
#5394=VECTOR('',#18723,10.);
#5395=VECTOR('',#18724,10.);
#5396=VECTOR('',#18727,10.);
#5397=VECTOR('',#18728,10.);
#5398=VECTOR('',#18731,10.);
#5399=VECTOR('',#18732,10.);
#5400=VECTOR('',#18735,10.);
#5401=VECTOR('',#18736,10.);
#5402=VECTOR('',#18739,10.);
#5403=VECTOR('',#18740,10.);
#5404=VECTOR('',#18743,10.);
#5405=VECTOR('',#18744,10.);
#5406=VECTOR('',#18747,10.);
#5407=VECTOR('',#18748,10.);
#5408=VECTOR('',#18751,10.);
#5409=VECTOR('',#18752,10.);
#5410=VECTOR('',#18755,10.);
#5411=VECTOR('',#18756,10.);
#5412=VECTOR('',#18759,10.);
#5413=VECTOR('',#18760,10.);
#5414=VECTOR('',#18763,10.);
#5415=VECTOR('',#18764,10.);
#5416=VECTOR('',#18767,10.);
#5417=VECTOR('',#18768,10.);
#5418=VECTOR('',#18771,10.);
#5419=VECTOR('',#18772,10.);
#5420=VECTOR('',#18775,10.);
#5421=VECTOR('',#18776,10.);
#5422=VECTOR('',#18779,10.);
#5423=VECTOR('',#18780,10.);
#5424=VECTOR('',#18783,10.);
#5425=VECTOR('',#18784,10.);
#5426=VECTOR('',#18787,10.);
#5427=VECTOR('',#18788,10.);
#5428=VECTOR('',#18791,10.);
#5429=VECTOR('',#18792,10.);
#5430=VECTOR('',#18795,10.);
#5431=VECTOR('',#18796,10.);
#5432=VECTOR('',#18799,10.);
#5433=VECTOR('',#18800,10.);
#5434=VECTOR('',#18803,10.);
#5435=VECTOR('',#18804,10.);
#5436=VECTOR('',#18807,10.);
#5437=VECTOR('',#18808,10.);
#5438=VECTOR('',#18811,10.);
#5439=VECTOR('',#18812,10.);
#5440=VECTOR('',#18815,10.);
#5441=VECTOR('',#18816,10.);
#5442=VECTOR('',#18819,10.);
#5443=VECTOR('',#18820,10.);
#5444=VECTOR('',#18823,10.);
#5445=VECTOR('',#18824,10.);
#5446=VECTOR('',#18827,10.);
#5447=VECTOR('',#18828,10.);
#5448=VECTOR('',#18835,2.31);
#5449=VECTOR('',#18840,10.);
#5450=VECTOR('',#18841,10.);
#5451=VECTOR('',#18842,10.);
#5452=VECTOR('',#18843,10.);
#5453=VECTOR('',#18844,10.);
#5454=VECTOR('',#18845,10.);
#5455=VECTOR('',#18848,10.);
#5456=VECTOR('',#18849,10.);
#5457=VECTOR('',#18850,10.);
#5458=VECTOR('',#18851,10.);
#5459=VECTOR('',#18854,10.);
#5460=VECTOR('',#18855,10.);
#5461=VECTOR('',#18856,10.);
#5462=VECTOR('',#18859,10.);
#5463=VECTOR('',#18860,10.);
#5464=VECTOR('',#18861,10.);
#5465=VECTOR('',#18862,10.);
#5466=VECTOR('',#18865,10.);
#5467=VECTOR('',#18866,10.);
#5468=VECTOR('',#18867,10.);
#5469=VECTOR('',#18870,10.);
#5470=VECTOR('',#18871,10.);
#5471=VECTOR('',#18874,10.);
#5472=VECTOR('',#18875,10.);
#5473=VECTOR('',#18878,10.);
#5474=VECTOR('',#18879,10.);
#5475=VECTOR('',#18882,10.);
#5476=VECTOR('',#18885,10.);
#5477=VECTOR('',#18892,10.);
#5478=VECTOR('',#18895,10.);
#5479=VECTOR('',#18992,6.25);
#5480=VECTOR('',#18997,2.);
#5481=VECTOR('',#19002,2.);
#5482=VECTOR('',#19005,2.);
#5483=VECTOR('',#19008,2.);
#5484=VECTOR('',#19011,2.);
#5485=VECTOR('',#19014,2.);
#5486=VECTOR('',#19017,2.);
#5487=VECTOR('',#19020,2.);
#5488=VECTOR('',#19023,2.);
#5489=VECTOR('',#19026,2.);
#5490=VECTOR('',#19029,2.);
#5491=VECTOR('',#19032,2.);
#5492=VECTOR('',#19035,2.);
#5493=VECTOR('',#19038,2.);
#5494=VECTOR('',#19041,2.);
#5495=VECTOR('',#19044,2.);
#5496=VECTOR('',#19047,2.);
#5497=VECTOR('',#19050,2.);
#5498=VECTOR('',#19053,2.);
#5499=VECTOR('',#19056,2.);
#5500=VECTOR('',#19059,2.);
#5501=VECTOR('',#19062,2.);
#5502=VECTOR('',#19065,2.);
#5503=VECTOR('',#19068,1.5555);
#5504=VECTOR('',#19073,1.5555);
#5505=VECTOR('',#19076,1.5555);
#5506=VECTOR('',#19079,1.5555);
#5507=VECTOR('',#19082,1.5555);
#5508=VECTOR('',#19085,1.5555);
#5509=VECTOR('',#19088,1.5555);
#5510=VECTOR('',#19091,1.5555);
#5511=VECTOR('',#19094,1.5555);
#5512=VECTOR('',#19097,1.5555);
#5513=VECTOR('',#19100,1.5555);
#5514=VECTOR('',#19103,1.5555);
#5515=VECTOR('',#19106,1.5555);
#5516=VECTOR('',#19109,1.5555);
#5517=VECTOR('',#19112,1.5555);
#5518=VECTOR('',#19115,1.5555);
#5519=VECTOR('',#19118,1.5555);
#5520=VECTOR('',#19121,1.5555);
#5521=VECTOR('',#19124,1.5555);
#5522=VECTOR('',#19127,1.5555);
#5523=VECTOR('',#19130,1.5555);
#5524=VECTOR('',#19133,1.5555);
#5525=VECTOR('',#19154,1.8);
#5526=VECTOR('',#19157,3.83322594216369);
#5527=VECTOR('',#19162,10.);
#5528=VECTOR('',#19163,10.);
#5529=VECTOR('',#19164,10.);
#5530=VECTOR('',#19167,10.);
#5531=VECTOR('',#19168,10.);
#5532=VECTOR('',#19171,10.);
#5533=VECTOR('',#19172,10.);
#5534=VECTOR('',#19175,10.);
#5535=VECTOR('',#19176,10.);
#5536=VECTOR('',#19179,10.);
#5537=VECTOR('',#19180,10.);
#5538=VECTOR('',#19183,10.);
#5539=VECTOR('',#19192,2.);
#5540=VECTOR('',#19197,2.);
#5541=VECTOR('',#19200,2.);
#5542=VECTOR('',#19203,2.);
#5543=VECTOR('',#19206,2.);
#5544=VECTOR('',#19209,2.);
#5545=VECTOR('',#19212,2.);
#5546=VECTOR('',#19215,2.);
#5547=VECTOR('',#19218,2.);
#5548=VECTOR('',#19221,2.);
#5549=VECTOR('',#19224,2.);
#5550=VECTOR('',#19227,2.);
#5551=VECTOR('',#19230,2.);
#5552=VECTOR('',#19233,2.);
#5553=VECTOR('',#19236,2.);
#5554=VECTOR('',#19239,2.);
#5555=VECTOR('',#19242,2.);
#5556=VECTOR('',#19245,2.);
#5557=VECTOR('',#19248,2.);
#5558=VECTOR('',#19251,2.);
#5559=VECTOR('',#19254,2.);
#5560=VECTOR('',#19257,2.);
#5561=VECTOR('',#19260,2.);
#5562=VECTOR('',#19263,2.);
#5563=VECTOR('',#19266,2.);
#5564=VECTOR('',#19269,2.);
#5565=VECTOR('',#19272,2.);
#5566=VECTOR('',#19275,2.);
#5567=VECTOR('',#19278,1.5555);
#5568=VECTOR('',#19283,1.5555);
#5569=VECTOR('',#19286,1.5555);
#5570=VECTOR('',#19289,1.5555);
#5571=VECTOR('',#19292,1.5555);
#5572=VECTOR('',#19295,1.5555);
#5573=VECTOR('',#19298,1.5555);
#5574=VECTOR('',#19301,1.5555);
#5575=VECTOR('',#19304,1.5555);
#5576=VECTOR('',#19307,1.5555);
#5577=VECTOR('',#19310,1.5555);
#5578=VECTOR('',#19313,1.5555);
#5579=VECTOR('',#19316,1.5555);
#5580=VECTOR('',#19319,1.5555);
#5581=VECTOR('',#19322,1.5555);
#5582=VECTOR('',#19325,1.5555);
#5583=VECTOR('',#19328,1.5555);
#5584=VECTOR('',#19331,1.5555);
#5585=VECTOR('',#19334,1.5555);
#5586=VECTOR('',#19337,1.5555);
#5587=VECTOR('',#19340,1.5555);
#5588=VECTOR('',#19343,1.5555);
#5589=VECTOR('',#19346,1.5555);
#5590=VECTOR('',#19349,1.5555);
#5591=VECTOR('',#19352,1.5555);
#5592=VECTOR('',#19355,1.5555);
#5593=VECTOR('',#19358,1.5555);
#5594=VECTOR('',#19361,1.5555);
#5595=VECTOR('',#19374,0.625);
#5596=VECTOR('',#19379,10.);
#5597=VECTOR('',#19380,10.);
#5598=VECTOR('',#19381,10.);
#5599=VECTOR('',#19384,10.);
#5600=VECTOR('',#19385,10.);
#5601=VECTOR('',#19388,10.);
#5602=VECTOR('',#19389,10.);
#5603=VECTOR('',#19392,10.);
#5604=VECTOR('',#19393,10.);
#5605=VECTOR('',#19396,10.);
#5606=VECTOR('',#19397,10.);
#5607=VECTOR('',#19400,10.);
#5608=VECTOR('',#19409,1.8);
#5609=VECTOR('',#19422,3.8);
#5610=VECTOR('',#19431,4.4);
#5611=VECTOR('',#19438,4.5);
#5612=VECTOR('',#19447,2.2);
#5613=VECTOR('',#19456,4.425);
#5614=VECTOR('',#19461,10.);
#5615=VECTOR('',#19462,10.);
#5616=VECTOR('',#19465,10.);
#5617=VECTOR('',#19468,3.83322594216369);
#5618=VECTOR('',#19475,2.15);
#5619=VECTOR('',#19480,2.05);
#5620=VECTOR('',#19491,2.15);
#5621=VECTOR('',#19496,10.);
#5622=VECTOR('',#19497,10.);
#5623=VECTOR('',#19500,10.);
#5624=VECTOR('',#19503,3.83322594216369);
#5625=VECTOR('',#19506,10.);
#5626=VECTOR('',#19509,10.);
#5627=VECTOR('',#19512,10.);
#5628=VECTOR('',#19515,10.);
#5629=VECTOR('',#19518,10.);
#5630=VECTOR('',#19521,10.);
#5631=VECTOR('',#19530,1.25);
#5632=VECTOR('',#19535,1.25);
#5633=VECTOR('',#19538,1.25);
#5634=VECTOR('',#19541,1.25);
#5635=VECTOR('',#19544,1.25);
#5636=VECTOR('',#19547,1.25);
#5637=VECTOR('',#19550,1.25);
#5638=VECTOR('',#19553,1.25);
#5639=VECTOR('',#19556,1.25);
#5640=VECTOR('',#19559,1.25);
#5641=VECTOR('',#19562,1.25);
#5642=VECTOR('',#19565,1.25);
#5643=VECTOR('',#19568,1.25);
#5644=VECTOR('',#19571,1.25);
#5645=VECTOR('',#19574,1.25);
#5646=VECTOR('',#19577,1.25);
#5647=VECTOR('',#19580,1.25);
#5648=VECTOR('',#19583,1.25);
#5649=VECTOR('',#19588,0.95825);
#5650=VECTOR('',#19593,0.95825);
#5651=VECTOR('',#19596,0.95825);
#5652=VECTOR('',#19599,0.95825);
#5653=VECTOR('',#19602,0.95825);
#5654=VECTOR('',#19605,0.95825);
#5655=VECTOR('',#19608,0.95825);
#5656=VECTOR('',#19611,0.95825);
#5657=VECTOR('',#19614,0.95825);
#5658=VECTOR('',#19617,0.95825);
#5659=VECTOR('',#19620,0.95825);
#5660=VECTOR('',#19623,0.95825);
#5661=VECTOR('',#19626,0.95825);
#5662=VECTOR('',#19629,0.95825);
#5663=VECTOR('',#19632,0.95825);
#5664=VECTOR('',#19635,0.95825);
#5665=VECTOR('',#19638,0.95825);
#5666=VECTOR('',#19651,0.375);
#5667=VECTOR('',#19656,10.);
#5668=VECTOR('',#19657,10.);
#5669=VECTOR('',#19658,10.);
#5670=VECTOR('',#19661,10.);
#5671=VECTOR('',#19662,10.);
#5672=VECTOR('',#19665,10.);
#5673=VECTOR('',#19666,10.);
#5674=VECTOR('',#19669,10.);
#5675=VECTOR('',#19670,10.);
#5676=VECTOR('',#19673,10.);
#5677=VECTOR('',#19674,10.);
#5678=VECTOR('',#19677,10.);
#5679=VECTOR('',#19686,1.125);
#5680=VECTOR('',#19699,2.35);
#5681=VERTEX_POINT('',#19751);
#5682=VERTEX_POINT('',#19752);
#5683=VERTEX_POINT('',#19754);
#5684=VERTEX_POINT('',#19756);
#5685=VERTEX_POINT('',#19758);
#5686=VERTEX_POINT('',#19762);
#5687=VERTEX_POINT('',#19768);
#5688=VERTEX_POINT('',#19772);
#5689=VERTEX_POINT('',#19774);
#5690=VERTEX_POINT('',#19778);
#5691=VERTEX_POINT('',#19780);
#5692=VERTEX_POINT('',#19784);
#5693=VERTEX_POINT('',#19790);
#5694=VERTEX_POINT('',#19794);
#5695=VERTEX_POINT('',#19798);
#5696=VERTEX_POINT('',#19799);
#5697=VERTEX_POINT('',#19801);
#5698=VERTEX_POINT('',#19805);
#5699=VERTEX_POINT('',#19806);
#5700=VERTEX_POINT('',#19811);
#5701=VERTEX_POINT('',#19813);
#5702=VERTEX_POINT('',#19817);
#5703=VERTEX_POINT('',#19818);
#5704=VERTEX_POINT('',#19826);
#5705=VERTEX_POINT('',#19835);
#5706=VERTEX_POINT('',#19836);
#5707=VERTEX_POINT('',#19840);
#5708=VERTEX_POINT('',#19842);
#5709=VERTEX_POINT('',#19846);
#5710=VERTEX_POINT('',#19848);
#5711=VERTEX_POINT('',#19855);
#5712=VERTEX_POINT('',#19857);
#5713=VERTEX_POINT('',#19859);
#5714=VERTEX_POINT('',#19861);
#5715=VERTEX_POINT('',#19863);
#5716=VERTEX_POINT('',#19871);
#5717=VERTEX_POINT('',#19875);
#5718=VERTEX_POINT('',#19880);
#5719=VERTEX_POINT('',#19883);
#5720=VERTEX_POINT('',#19884);
#5721=VERTEX_POINT('',#19886);
#5722=VERTEX_POINT('',#19893);
#5723=VERTEX_POINT('',#19895);
#5724=VERTEX_POINT('',#19899);
#5725=VERTEX_POINT('',#19903);
#5726=VERTEX_POINT('',#19904);
#5727=VERTEX_POINT('',#19914);
#5728=VERTEX_POINT('',#19918);
#5729=VERTEX_POINT('',#19922);
#5730=VERTEX_POINT('',#19931);
#5731=VERTEX_POINT('',#19932);
#5732=VERTEX_POINT('',#19937);
#5733=VERTEX_POINT('',#19939);
#5734=VERTEX_POINT('',#19943);
#5735=VERTEX_POINT('',#19944);
#5736=VERTEX_POINT('',#19952);
#5737=VERTEX_POINT('',#19955);
#5738=VERTEX_POINT('',#19961);
#5739=VERTEX_POINT('',#19970);
#5740=VERTEX_POINT('',#19974);
#5741=VERTEX_POINT('',#19986);
#5742=VERTEX_POINT('',#19987);
#5743=VERTEX_POINT('',#19989);
#5744=VERTEX_POINT('',#19991);
#5745=VERTEX_POINT('',#19995);
#5746=VERTEX_POINT('',#19997);
#5747=VERTEX_POINT('',#20001);
#5748=VERTEX_POINT('',#20002);
#5749=VERTEX_POINT('',#20007);
#5750=VERTEX_POINT('',#20009);
#5751=VERTEX_POINT('',#20013);
#5752=VERTEX_POINT('',#20015);
#5753=VERTEX_POINT('',#20019);
#5754=VERTEX_POINT('',#20021);
#5755=VERTEX_POINT('',#20028);
#5756=VERTEX_POINT('',#20031);
#5757=VERTEX_POINT('',#20035);
#5758=VERTEX_POINT('',#20037);
#5759=VERTEX_POINT('',#20043);
#5760=VERTEX_POINT('',#20044);
#5761=VERTEX_POINT('',#20046);
#5762=VERTEX_POINT('',#20048);
#5763=VERTEX_POINT('',#20052);
#5764=VERTEX_POINT('',#20053);
#5765=VERTEX_POINT('',#20055);
#5766=VERTEX_POINT('',#20057);
#5767=VERTEX_POINT('',#20061);
#5768=VERTEX_POINT('',#20063);
#5769=VERTEX_POINT('',#20067);
#5770=VERTEX_POINT('',#20068);
#5771=VERTEX_POINT('',#20073);
#5772=VERTEX_POINT('',#20074);
#5773=VERTEX_POINT('',#20077);
#5774=VERTEX_POINT('',#20081);
#5775=VERTEX_POINT('',#20082);
#5776=VERTEX_POINT('',#20087);
#5777=VERTEX_POINT('',#20088);
#5778=VERTEX_POINT('',#20093);
#5779=VERTEX_POINT('',#20094);
#5780=VERTEX_POINT('',#20102);
#5781=VERTEX_POINT('',#20104);
#5782=VERTEX_POINT('',#20108);
#5783=VERTEX_POINT('',#20109);
#5784=VERTEX_POINT('',#20112);
#5785=VERTEX_POINT('',#20116);
#5786=VERTEX_POINT('',#20118);
#5787=VERTEX_POINT('',#20120);
#5788=VERTEX_POINT('',#20122);
#5789=VERTEX_POINT('',#20124);
#5790=VERTEX_POINT('',#20126);
#5791=VERTEX_POINT('',#20128);
#5792=VERTEX_POINT('',#20130);
#5793=VERTEX_POINT('',#20132);
#5794=VERTEX_POINT('',#20134);
#5795=VERTEX_POINT('',#20136);
#5796=VERTEX_POINT('',#20147);
#5797=VERTEX_POINT('',#20149);
#5798=VERTEX_POINT('',#20151);
#5799=VERTEX_POINT('',#20153);
#5800=VERTEX_POINT('',#20155);
#5801=VERTEX_POINT('',#20157);
#5802=VERTEX_POINT('',#20159);
#5803=VERTEX_POINT('',#20161);
#5804=VERTEX_POINT('',#20163);
#5805=VERTEX_POINT('',#20165);
#5806=VERTEX_POINT('',#20169);
#5807=VERTEX_POINT('',#20171);
#5808=VERTEX_POINT('',#20173);
#5809=VERTEX_POINT('',#20179);
#5810=VERTEX_POINT('',#20181);
#5811=VERTEX_POINT('',#20187);
#5812=VERTEX_POINT('',#20189);
#5813=VERTEX_POINT('',#20191);
#5814=VERTEX_POINT('',#20195);
#5815=VERTEX_POINT('',#20201);
#5816=VERTEX_POINT('',#20203);
#5817=VERTEX_POINT('',#20207);
#5818=VERTEX_POINT('',#20208);
#5819=VERTEX_POINT('',#20211);
#5820=VERTEX_POINT('',#20215);
#5821=VERTEX_POINT('',#20219);
#5822=VERTEX_POINT('',#20223);
#5823=VERTEX_POINT('',#20227);
#5824=VERTEX_POINT('',#20228);
#5825=VERTEX_POINT('',#20235);
#5826=VERTEX_POINT('',#20237);
#5827=VERTEX_POINT('',#20246);
#5828=VERTEX_POINT('',#20248);
#5829=VERTEX_POINT('',#20255);
#5830=VERTEX_POINT('',#20258);
#5831=VERTEX_POINT('',#20262);
#5832=VERTEX_POINT('',#20270);
#5833=VERTEX_POINT('',#20274);
#5834=VERTEX_POINT('',#20278);
#5835=VERTEX_POINT('',#20279);
#5836=VERTEX_POINT('',#20284);
#5837=VERTEX_POINT('',#20286);
#5838=VERTEX_POINT('',#20290);
#5839=VERTEX_POINT('',#20298);
#5840=VERTEX_POINT('',#20301);
#5841=VERTEX_POINT('',#20304);
#5842=VERTEX_POINT('',#20313);
#5843=VERTEX_POINT('',#20314);
#5844=VERTEX_POINT('',#20319);
#5845=VERTEX_POINT('',#20320);
#5846=VERTEX_POINT('',#20325);
#5847=VERTEX_POINT('',#20332);
#5848=VERTEX_POINT('',#20339);
#5849=VERTEX_POINT('',#20343);
#5850=VERTEX_POINT('',#20345);
#5851=VERTEX_POINT('',#20352);
#5852=VERTEX_POINT('',#20360);
#5853=VERTEX_POINT('',#20367);
#5854=VERTEX_POINT('',#20368);
#5855=VERTEX_POINT('',#20370);
#5856=VERTEX_POINT('',#20372);
#5857=VERTEX_POINT('',#20378);
#5858=VERTEX_POINT('',#20383);
#5859=VERTEX_POINT('',#20390);
#5860=VERTEX_POINT('',#20395);
#5861=VERTEX_POINT('',#20402);
#5862=VERTEX_POINT('',#20403);
#5863=VERTEX_POINT('',#20412);
#5864=VERTEX_POINT('',#20416);
#5865=VERTEX_POINT('',#20422);
#5866=VERTEX_POINT('',#20424);
#5867=VERTEX_POINT('',#20426);
#5868=VERTEX_POINT('',#20428);
#5869=VERTEX_POINT('',#20432);
#5870=VERTEX_POINT('',#20436);
#5871=VERTEX_POINT('',#20437);
#5872=VERTEX_POINT('',#20439);
#5873=VERTEX_POINT('',#20444);
#5874=VERTEX_POINT('',#20451);
#5875=VERTEX_POINT('',#20452);
#5876=VERTEX_POINT('',#20454);
#5877=VERTEX_POINT('',#20459);
#5878=VERTEX_POINT('',#20475);
#5879=VERTEX_POINT('',#20479);
#5880=VERTEX_POINT('',#20485);
#5881=VERTEX_POINT('',#20495);
#5882=VERTEX_POINT('',#20504);
#5883=VERTEX_POINT('',#20508);
#5884=VERTEX_POINT('',#20525);
#5885=VERTEX_POINT('',#20526);
#5886=VERTEX_POINT('',#20528);
#5887=VERTEX_POINT('',#20530);
#5888=VERTEX_POINT('',#20534);
#5889=VERTEX_POINT('',#20535);
#5890=VERTEX_POINT('',#20540);
#5891=VERTEX_POINT('',#20541);
#5892=VERTEX_POINT('',#20546);
#5893=VERTEX_POINT('',#20548);
#5894=VERTEX_POINT('',#20552);
#5895=VERTEX_POINT('',#20556);
#5896=VERTEX_POINT('',#20560);
#5897=VERTEX_POINT('',#20562);
#5898=VERTEX_POINT('',#20566);
#5899=VERTEX_POINT('',#20570);
#5900=VERTEX_POINT('',#20575);
#5901=VERTEX_POINT('',#20576);
#5902=VERTEX_POINT('',#20578);
#5903=VERTEX_POINT('',#20580);
#5904=VERTEX_POINT('',#20582);
#5905=VERTEX_POINT('',#20584);
#5906=VERTEX_POINT('',#20588);
#5907=VERTEX_POINT('',#20589);
#5908=VERTEX_POINT('',#20591);
#5909=VERTEX_POINT('',#20593);
#5910=VERTEX_POINT('',#20597);
#5911=VERTEX_POINT('',#20598);
#5912=VERTEX_POINT('',#20603);
#5913=VERTEX_POINT('',#20604);
#5914=VERTEX_POINT('',#20609);
#5915=VERTEX_POINT('',#20611);
#5916=VERTEX_POINT('',#20615);
#5917=VERTEX_POINT('',#20619);
#5918=VERTEX_POINT('',#20623);
#5919=VERTEX_POINT('',#20624);
#5920=VERTEX_POINT('',#20626);
#5921=VERTEX_POINT('',#20630);
#5922=VERTEX_POINT('',#20631);
#5923=VERTEX_POINT('',#20636);
#5924=VERTEX_POINT('',#20637);
#5925=VERTEX_POINT('',#20640);
#5926=VERTEX_POINT('',#20644);
#5927=VERTEX_POINT('',#20645);
#5928=VERTEX_POINT('',#20648);
#5929=VERTEX_POINT('',#20652);
#5930=VERTEX_POINT('',#20656);
#5931=VERTEX_POINT('',#20660);
#5932=VERTEX_POINT('',#20662);
#5933=VERTEX_POINT('',#20666);
#5934=VERTEX_POINT('',#20668);
#5935=VERTEX_POINT('',#20672);
#5936=VERTEX_POINT('',#20678);
#5937=VERTEX_POINT('',#20680);
#5938=VERTEX_POINT('',#20684);
#5939=VERTEX_POINT('',#20690);
#5940=VERTEX_POINT('',#20694);
#5941=VERTEX_POINT('',#20695);
#5942=VERTEX_POINT('',#20697);
#5943=VERTEX_POINT('',#20699);
#5944=VERTEX_POINT('',#20701);
#5945=VERTEX_POINT('',#20703);
#5946=VERTEX_POINT('',#20707);
#5947=VERTEX_POINT('',#20709);
#5948=VERTEX_POINT('',#20713);
#5949=VERTEX_POINT('',#20717);
#5950=VERTEX_POINT('',#20719);
#5951=VERTEX_POINT('',#20723);
#5952=VERTEX_POINT('',#20738);
#5953=VERTEX_POINT('',#20742);
#5954=VERTEX_POINT('',#20743);
#5955=VERTEX_POINT('',#20745);
#5956=VERTEX_POINT('',#20747);
#5957=VERTEX_POINT('',#20749);
#5958=VERTEX_POINT('',#20751);
#5959=VERTEX_POINT('',#20755);
#5960=VERTEX_POINT('',#20757);
#5961=VERTEX_POINT('',#20761);
#5962=VERTEX_POINT('',#20765);
#5963=VERTEX_POINT('',#20769);
#5964=VERTEX_POINT('',#20770);
#5965=VERTEX_POINT('',#20772);
#5966=VERTEX_POINT('',#20774);
#5967=VERTEX_POINT('',#20778);
#5968=VERTEX_POINT('',#20780);
#5969=VERTEX_POINT('',#20784);
#5970=VERTEX_POINT('',#20785);
#5971=VERTEX_POINT('',#20787);
#5972=VERTEX_POINT('',#20789);
#5973=VERTEX_POINT('',#20793);
#5974=VERTEX_POINT('',#20795);
#5975=VERTEX_POINT('',#20814);
#5976=VERTEX_POINT('',#20815);
#5977=VERTEX_POINT('',#20817);
#5978=VERTEX_POINT('',#20821);
#5979=VERTEX_POINT('',#20822);
#5980=VERTEX_POINT('',#20827);
#5981=VERTEX_POINT('',#20828);
#5982=VERTEX_POINT('',#20830);
#5983=VERTEX_POINT('',#20834);
#5984=VERTEX_POINT('',#20835);
#5985=VERTEX_POINT('',#20840);
#5986=VERTEX_POINT('',#20841);
#5987=VERTEX_POINT('',#20844);
#5988=VERTEX_POINT('',#20851);
#5989=VERTEX_POINT('',#20852);
#5990=VERTEX_POINT('',#20855);
#5991=VERTEX_POINT('',#20861);
#5992=VERTEX_POINT('',#20865);
#5993=VERTEX_POINT('',#20867);
#5994=VERTEX_POINT('',#20871);
#5995=VERTEX_POINT('',#20872);
#5996=VERTEX_POINT('',#20874);
#5997=VERTEX_POINT('',#20878);
#5998=VERTEX_POINT('',#20879);
#5999=VERTEX_POINT('',#20884);
#6000=VERTEX_POINT('',#20885);
#6001=VERTEX_POINT('',#20887);
#6002=VERTEX_POINT('',#20891);
#6003=VERTEX_POINT('',#20892);
#6004=VERTEX_POINT('',#20897);
#6005=VERTEX_POINT('',#20898);
#6006=VERTEX_POINT('',#20901);
#6007=VERTEX_POINT('',#20908);
#6008=VERTEX_POINT('',#20909);
#6009=VERTEX_POINT('',#20912);
#6010=VERTEX_POINT('',#20918);
#6011=VERTEX_POINT('',#20922);
#6012=VERTEX_POINT('',#20924);
#6013=VERTEX_POINT('',#20928);
#6014=VERTEX_POINT('',#20930);
#6015=VERTEX_POINT('',#20932);
#6016=VERTEX_POINT('',#20936);
#6017=VERTEX_POINT('',#20940);
#6018=VERTEX_POINT('',#20942);
#6019=VERTEX_POINT('',#20946);
#6020=VERTEX_POINT('',#20947);
#6021=VERTEX_POINT('',#20949);
#6022=VERTEX_POINT('',#20951);
#6023=VERTEX_POINT('',#20955);
#6024=VERTEX_POINT('',#20957);
#6025=VERTEX_POINT('',#20961);
#6026=VERTEX_POINT('',#20963);
#6027=VERTEX_POINT('',#20967);
#6028=VERTEX_POINT('',#20971);
#6029=VERTEX_POINT('',#20973);
#6030=VERTEX_POINT('',#20980);
#6031=VERTEX_POINT('',#20981);
#6032=VERTEX_POINT('',#20983);
#6033=VERTEX_POINT('',#20985);
#6034=VERTEX_POINT('',#20987);
#6035=VERTEX_POINT('',#20990);
#6036=VERTEX_POINT('',#20992);
#6037=VERTEX_POINT('',#20995);
#6038=VERTEX_POINT('',#20997);
#6039=VERTEX_POINT('',#21000);
#6040=VERTEX_POINT('',#21002);
#6041=VERTEX_POINT('',#21004);
#6042=VERTEX_POINT('',#21006);
#6043=VERTEX_POINT('',#21008);
#6044=VERTEX_POINT('',#21012);
#6045=VERTEX_POINT('',#21014);
#6046=VERTEX_POINT('',#21018);
#6047=VERTEX_POINT('',#21019);
#6048=VERTEX_POINT('',#21024);
#6049=VERTEX_POINT('',#21025);
#6050=VERTEX_POINT('',#21030);
#6051=VERTEX_POINT('',#21031);
#6052=VERTEX_POINT('',#21036);
#6053=VERTEX_POINT('',#21037);
#6054=VERTEX_POINT('',#21042);
#6055=VERTEX_POINT('',#21043);
#6056=VERTEX_POINT('',#21048);
#6057=VERTEX_POINT('',#21049);
#6058=VERTEX_POINT('',#21057);
#6059=VERTEX_POINT('',#21059);
#6060=VERTEX_POINT('',#21063);
#6061=VERTEX_POINT('',#21066);
#6062=VERTEX_POINT('',#21069);
#6063=VERTEX_POINT('',#21074);
#6064=VERTEX_POINT('',#21088);
#6065=VERTEX_POINT('',#21092);
#6066=VERTEX_POINT('',#21099);
#6067=VERTEX_POINT('',#21103);
#6068=VERTEX_POINT('',#21105);
#6069=VERTEX_POINT('',#21109);
#6070=VERTEX_POINT('',#21110);
#6071=VERTEX_POINT('',#21115);
#6072=VERTEX_POINT('',#21117);
#6073=VERTEX_POINT('',#21121);
#6074=VERTEX_POINT('',#21126);
#6075=VERTEX_POINT('',#21130);
#6076=VERTEX_POINT('',#21134);
#6077=VERTEX_POINT('',#21158);
#6078=VERTEX_POINT('',#21163);
#6079=VERTEX_POINT('',#21205);
#6080=VERTEX_POINT('',#21207);
#6081=VERTEX_POINT('',#21216);
#6082=VERTEX_POINT('',#21218);
#6083=VERTEX_POINT('',#21220);
#6084=VERTEX_POINT('',#21264);
#6085=VERTEX_POINT('',#21291);
#6086=VERTEX_POINT('',#21293);
#6087=VERTEX_POINT('',#21295);
#6088=VERTEX_POINT('',#21305);
#6089=VERTEX_POINT('',#21307);
#6090=VERTEX_POINT('',#21351);
#6091=VERTEX_POINT('',#21355);
#6092=VERTEX_POINT('',#21359);
#6093=VERTEX_POINT('',#21363);
#6094=VERTEX_POINT('',#21367);
#6095=VERTEX_POINT('',#21388);
#6096=VERTEX_POINT('',#21390);
#6097=VERTEX_POINT('',#21394);
#6098=VERTEX_POINT('',#21398);
#6099=VERTEX_POINT('',#21399);
#6100=VERTEX_POINT('',#21401);
#6101=VERTEX_POINT('',#21403);
#6102=VERTEX_POINT('',#21405);
#6103=VERTEX_POINT('',#21407);
#6104=VERTEX_POINT('',#21409);
#6105=VERTEX_POINT('',#21411);
#6106=VERTEX_POINT('',#21414);
#6107=VERTEX_POINT('',#21416);
#6108=VERTEX_POINT('',#21419);
#6109=VERTEX_POINT('',#21423);
#6110=VERTEX_POINT('',#21424);
#6111=VERTEX_POINT('',#21426);
#6112=VERTEX_POINT('',#21428);
#6113=VERTEX_POINT('',#21430);
#6114=VERTEX_POINT('',#21432);
#6115=VERTEX_POINT('',#21434);
#6116=VERTEX_POINT('',#21436);
#6117=VERTEX_POINT('',#21439);
#6118=VERTEX_POINT('',#21441);
#6119=VERTEX_POINT('',#21444);
#6120=VERTEX_POINT('',#21446);
#6121=VERTEX_POINT('',#21450);
#6122=VERTEX_POINT('',#21454);
#6123=VERTEX_POINT('',#21458);
#6124=VERTEX_POINT('',#21462);
#6125=VERTEX_POINT('',#21466);
#6126=VERTEX_POINT('',#21470);
#6127=VERTEX_POINT('',#21476);
#6128=VERTEX_POINT('',#21478);
#6129=VERTEX_POINT('',#21482);
#6130=VERTEX_POINT('',#21486);
#6131=VERTEX_POINT('',#21490);
#6132=VERTEX_POINT('',#21494);
#6133=VERTEX_POINT('',#21496);
#6134=VERTEX_POINT('',#21498);
#6135=VERTEX_POINT('',#21502);
#6136=VERTEX_POINT('',#21506);
#6137=VERTEX_POINT('',#21510);
#6138=VERTEX_POINT('',#21514);
#6139=VERTEX_POINT('',#21518);
#6140=VERTEX_POINT('',#21519);
#6141=VERTEX_POINT('',#21524);
#6142=VERTEX_POINT('',#21525);
#6143=VERTEX_POINT('',#21533);
#6144=VERTEX_POINT('',#21535);
#6145=VERTEX_POINT('',#21539);
#6146=VERTEX_POINT('',#21543);
#6147=VERTEX_POINT('',#21547);
#6148=VERTEX_POINT('',#21562);
#6149=VERTEX_POINT('',#21566);
#6150=VERTEX_POINT('',#21570);
#6151=VERTEX_POINT('',#21593);
#6152=VERTEX_POINT('',#21594);
#6153=VERTEX_POINT('',#21596);
#6154=VERTEX_POINT('',#21598);
#6155=VERTEX_POINT('',#21602);
#6156=VERTEX_POINT('',#21604);
#6157=VERTEX_POINT('',#21608);
#6158=VERTEX_POINT('',#21610);
#6159=VERTEX_POINT('',#21618);
#6160=VERTEX_POINT('',#21619);
#6161=VERTEX_POINT('',#21621);
#6162=VERTEX_POINT('',#21623);
#6163=VERTEX_POINT('',#21627);
#6164=VERTEX_POINT('',#21629);
#6165=VERTEX_POINT('',#21633);
#6166=VERTEX_POINT('',#21635);
#6167=VERTEX_POINT('',#21643);
#6168=VERTEX_POINT('',#21644);
#6169=VERTEX_POINT('',#21646);
#6170=VERTEX_POINT('',#21648);
#6171=VERTEX_POINT('',#21652);
#6172=VERTEX_POINT('',#21654);
#6173=VERTEX_POINT('',#21658);
#6174=VERTEX_POINT('',#21660);
#6175=VERTEX_POINT('',#21668);
#6176=VERTEX_POINT('',#21669);
#6177=VERTEX_POINT('',#21671);
#6178=VERTEX_POINT('',#21673);
#6179=VERTEX_POINT('',#21677);
#6180=VERTEX_POINT('',#21679);
#6181=VERTEX_POINT('',#21683);
#6182=VERTEX_POINT('',#21685);
#6183=VERTEX_POINT('',#21695);
#6184=VERTEX_POINT('',#21696);
#6185=VERTEX_POINT('',#21698);
#6186=VERTEX_POINT('',#21702);
#6187=VERTEX_POINT('',#21703);
#6188=VERTEX_POINT('',#21705);
#6189=VERTEX_POINT('',#21709);
#6190=VERTEX_POINT('',#21710);
#6191=VERTEX_POINT('',#21712);
#6192=VERTEX_POINT('',#21716);
#6193=VERTEX_POINT('',#21717);
#6194=VERTEX_POINT('',#21719);
#6195=VERTEX_POINT('',#21723);
#6196=VERTEX_POINT('',#21724);
#6197=VERTEX_POINT('',#21726);
#6198=VERTEX_POINT('',#21730);
#6199=VERTEX_POINT('',#21731);
#6200=VERTEX_POINT('',#21733);
#6201=VERTEX_POINT('',#21737);
#6202=VERTEX_POINT('',#21738);
#6203=VERTEX_POINT('',#21740);
#6204=VERTEX_POINT('',#21747);
#6205=VERTEX_POINT('',#21748);
#6206=VERTEX_POINT('',#21750);
#6207=VERTEX_POINT('',#21789);
#6208=VERTEX_POINT('',#21793);
#6209=VERTEX_POINT('',#21800);
#6210=VERTEX_POINT('',#21801);
#6211=VERTEX_POINT('',#21803);
#6212=VERTEX_POINT('',#21814);
#6213=VERTEX_POINT('',#21824);
#6214=VERTEX_POINT('',#21825);
#6215=VERTEX_POINT('',#21872);
#6216=VERTEX_POINT('',#21873);
#6217=VERTEX_POINT('',#21920);
#6218=VERTEX_POINT('',#21921);
#6219=VERTEX_POINT('',#21974);
#6220=VERTEX_POINT('',#21975);
#6221=VERTEX_POINT('',#22022);
#6222=VERTEX_POINT('',#22023);
#6223=VERTEX_POINT('',#22070);
#6224=VERTEX_POINT('',#22071);
#6225=VERTEX_POINT('',#22124);
#6226=VERTEX_POINT('',#22125);
#6227=VERTEX_POINT('',#22172);
#6228=VERTEX_POINT('',#22173);
#6229=VERTEX_POINT('',#22220);
#6230=VERTEX_POINT('',#22221);
#6231=VERTEX_POINT('',#22268);
#6232=VERTEX_POINT('',#22269);
#6233=VERTEX_POINT('',#22322);
#6234=VERTEX_POINT('',#22323);
#6235=VERTEX_POINT('',#22370);
#6236=VERTEX_POINT('',#22371);
#6237=VERTEX_POINT('',#22418);
#6238=VERTEX_POINT('',#22419);
#6239=VERTEX_POINT('',#22472);
#6240=VERTEX_POINT('',#22473);
#6241=VERTEX_POINT('',#22520);
#6242=VERTEX_POINT('',#22521);
#6243=VERTEX_POINT('',#22568);
#6244=VERTEX_POINT('',#22569);
#6245=VERTEX_POINT('',#22622);
#6246=VERTEX_POINT('',#22623);
#6247=VERTEX_POINT('',#22670);
#6248=VERTEX_POINT('',#22671);
#6249=VERTEX_POINT('',#22718);
#6250=VERTEX_POINT('',#22719);
#6251=VERTEX_POINT('',#22772);
#6252=VERTEX_POINT('',#22773);
#6253=VERTEX_POINT('',#22820);
#6254=VERTEX_POINT('',#22821);
#6255=VERTEX_POINT('',#22868);
#6256=VERTEX_POINT('',#22869);
#6257=VERTEX_POINT('',#22922);
#6258=VERTEX_POINT('',#22923);
#6259=VERTEX_POINT('',#22970);
#6260=VERTEX_POINT('',#22971);
#6261=VERTEX_POINT('',#23018);
#6262=VERTEX_POINT('',#23019);
#6263=VERTEX_POINT('',#23072);
#6264=VERTEX_POINT('',#23073);
#6265=VERTEX_POINT('',#23120);
#6266=VERTEX_POINT('',#23121);
#6267=VERTEX_POINT('',#23168);
#6268=VERTEX_POINT('',#23169);
#6269=VERTEX_POINT('',#23171);
#6270=VERTEX_POINT('',#23181);
#6271=VERTEX_POINT('',#23192);
#6272=VERTEX_POINT('',#23193);
#6273=VERTEX_POINT('',#23216);
#6274=VERTEX_POINT('',#23217);
#6275=VERTEX_POINT('',#23241);
#6276=VERTEX_POINT('',#23242);
#6277=VERTEX_POINT('',#23266);
#6278=VERTEX_POINT('',#23267);
#6279=VERTEX_POINT('',#23290);
#6280=VERTEX_POINT('',#23291);
#6281=VERTEX_POINT('',#23315);
#6282=VERTEX_POINT('',#23316);
#6283=VERTEX_POINT('',#23340);
#6284=VERTEX_POINT('',#23341);
#6285=VERTEX_POINT('',#23364);
#6286=VERTEX_POINT('',#23365);
#6287=VERTEX_POINT('',#23389);
#6288=VERTEX_POINT('',#23390);
#6289=VERTEX_POINT('',#23414);
#6290=VERTEX_POINT('',#23415);
#6291=VERTEX_POINT('',#23438);
#6292=VERTEX_POINT('',#23439);
#6293=VERTEX_POINT('',#23463);
#6294=VERTEX_POINT('',#23464);
#6295=VERTEX_POINT('',#23488);
#6296=VERTEX_POINT('',#23489);
#6297=VERTEX_POINT('',#23512);
#6298=VERTEX_POINT('',#23513);
#6299=VERTEX_POINT('',#23537);
#6300=VERTEX_POINT('',#23538);
#6301=VERTEX_POINT('',#23562);
#6302=VERTEX_POINT('',#23563);
#6303=VERTEX_POINT('',#23586);
#6304=VERTEX_POINT('',#23587);
#6305=VERTEX_POINT('',#23611);
#6306=VERTEX_POINT('',#23612);
#6307=VERTEX_POINT('',#23636);
#6308=VERTEX_POINT('',#23637);
#6309=VERTEX_POINT('',#23660);
#6310=VERTEX_POINT('',#23661);
#6311=VERTEX_POINT('',#23684);
#6312=VERTEX_POINT('',#23685);
#6313=VERTEX_POINT('',#23709);
#6314=VERTEX_POINT('',#23710);
#6315=VERTEX_POINT('',#23734);
#6316=VERTEX_POINT('',#23735);
#6317=VERTEX_POINT('',#23758);
#6318=VERTEX_POINT('',#23759);
#6319=VERTEX_POINT('',#23783);
#6320=VERTEX_POINT('',#23784);
#6321=VERTEX_POINT('',#23808);
#6322=VERTEX_POINT('',#23809);
#6323=VERTEX_POINT('',#23832);
#6324=VERTEX_POINT('',#23833);
#6325=VERTEX_POINT('',#23835);
#6326=VERTEX_POINT('',#23838);
#6327=VERTEX_POINT('',#23840);
#6328=VERTEX_POINT('',#23842);
#6329=VERTEX_POINT('',#23844);
#6330=VERTEX_POINT('',#23846);
#6331=VERTEX_POINT('',#23848);
#6332=VERTEX_POINT('',#23850);
#6333=VERTEX_POINT('',#23852);
#6334=VERTEX_POINT('',#23854);
#6335=VERTEX_POINT('',#23856);
#6336=VERTEX_POINT('',#23858);
#6337=VERTEX_POINT('',#23860);
#6338=VERTEX_POINT('',#23862);
#6339=VERTEX_POINT('',#23864);
#6340=VERTEX_POINT('',#23866);
#6341=VERTEX_POINT('',#23868);
#6342=VERTEX_POINT('',#23870);
#6343=VERTEX_POINT('',#23872);
#6344=VERTEX_POINT('',#23874);
#6345=VERTEX_POINT('',#23876);
#6346=VERTEX_POINT('',#23878);
#6347=VERTEX_POINT('',#23880);
#6348=VERTEX_POINT('',#23882);
#6349=VERTEX_POINT('',#23884);
#6350=VERTEX_POINT('',#23886);
#6351=VERTEX_POINT('',#23888);
#6352=VERTEX_POINT('',#23890);
#6353=VERTEX_POINT('',#23892);
#6354=VERTEX_POINT('',#23894);
#6355=VERTEX_POINT('',#23896);
#6356=VERTEX_POINT('',#23898);
#6357=VERTEX_POINT('',#23900);
#6358=VERTEX_POINT('',#23902);
#6359=VERTEX_POINT('',#23904);
#6360=VERTEX_POINT('',#23906);
#6361=VERTEX_POINT('',#23908);
#6362=VERTEX_POINT('',#23910);
#6363=VERTEX_POINT('',#23912);
#6364=VERTEX_POINT('',#23914);
#6365=VERTEX_POINT('',#23916);
#6366=VERTEX_POINT('',#23918);
#6367=VERTEX_POINT('',#23920);
#6368=VERTEX_POINT('',#23922);
#6369=VERTEX_POINT('',#23924);
#6370=VERTEX_POINT('',#23926);
#6371=VERTEX_POINT('',#23928);
#6372=VERTEX_POINT('',#23930);
#6373=VERTEX_POINT('',#23934);
#6374=VERTEX_POINT('',#23936);
#6375=VERTEX_POINT('',#23938);
#6376=VERTEX_POINT('',#23941);
#6377=VERTEX_POINT('',#23943);
#6378=VERTEX_POINT('',#23946);
#6379=VERTEX_POINT('',#23948);
#6380=VERTEX_POINT('',#23951);
#6381=VERTEX_POINT('',#23953);
#6382=VERTEX_POINT('',#23956);
#6383=VERTEX_POINT('',#23958);
#6384=VERTEX_POINT('',#23961);
#6385=VERTEX_POINT('',#23963);
#6386=VERTEX_POINT('',#23966);
#6387=VERTEX_POINT('',#23968);
#6388=VERTEX_POINT('',#23971);
#6389=VERTEX_POINT('',#23973);
#6390=VERTEX_POINT('',#23976);
#6391=VERTEX_POINT('',#23978);
#6392=VERTEX_POINT('',#23981);
#6393=VERTEX_POINT('',#23983);
#6394=VERTEX_POINT('',#23986);
#6395=VERTEX_POINT('',#23988);
#6396=VERTEX_POINT('',#23991);
#6397=VERTEX_POINT('',#23993);
#6398=VERTEX_POINT('',#23996);
#6399=VERTEX_POINT('',#23998);
#6400=VERTEX_POINT('',#24001);
#6401=VERTEX_POINT('',#24003);
#6402=VERTEX_POINT('',#24006);
#6403=VERTEX_POINT('',#24008);
#6404=VERTEX_POINT('',#24011);
#6405=VERTEX_POINT('',#24013);
#6406=VERTEX_POINT('',#24016);
#6407=VERTEX_POINT('',#24018);
#6408=VERTEX_POINT('',#24021);
#6409=VERTEX_POINT('',#24023);
#6410=VERTEX_POINT('',#24026);
#6411=VERTEX_POINT('',#24028);
#6412=VERTEX_POINT('',#24031);
#6413=VERTEX_POINT('',#24033);
#6414=VERTEX_POINT('',#24036);
#6415=VERTEX_POINT('',#24038);
#6416=VERTEX_POINT('',#24041);
#6417=VERTEX_POINT('',#24043);
#6418=VERTEX_POINT('',#24046);
#6419=VERTEX_POINT('',#24048);
#6420=VERTEX_POINT('',#24051);
#6421=VERTEX_POINT('',#24053);
#6422=VERTEX_POINT('',#24056);
#6423=VERTEX_POINT('',#24060);
#6424=VERTEX_POINT('',#24061);
#6425=VERTEX_POINT('',#24983);
#6426=VERTEX_POINT('',#25091);
#6427=VERTEX_POINT('',#25094);
#6428=VERTEX_POINT('',#25926);
#6429=VERTEX_POINT('',#25928);
#6430=VERTEX_POINT('',#25937);
#6431=VERTEX_POINT('',#25939);
#6432=VERTEX_POINT('',#25948);
#6433=VERTEX_POINT('',#25950);
#6434=VERTEX_POINT('',#25959);
#6435=VERTEX_POINT('',#25961);
#6436=VERTEX_POINT('',#25970);
#6437=VERTEX_POINT('',#25972);
#6438=VERTEX_POINT('',#25981);
#6439=VERTEX_POINT('',#25983);
#6440=VERTEX_POINT('',#25992);
#6441=VERTEX_POINT('',#25994);
#6442=VERTEX_POINT('',#26003);
#6443=VERTEX_POINT('',#26005);
#6444=VERTEX_POINT('',#26014);
#6445=VERTEX_POINT('',#26016);
#6446=VERTEX_POINT('',#26025);
#6447=VERTEX_POINT('',#26027);
#6448=VERTEX_POINT('',#26036);
#6449=VERTEX_POINT('',#26038);
#6450=VERTEX_POINT('',#26047);
#6451=VERTEX_POINT('',#26049);
#6452=VERTEX_POINT('',#26058);
#6453=VERTEX_POINT('',#26060);
#6454=VERTEX_POINT('',#26069);
#6455=VERTEX_POINT('',#26071);
#6456=VERTEX_POINT('',#26080);
#6457=VERTEX_POINT('',#26082);
#6458=VERTEX_POINT('',#26091);
#6459=VERTEX_POINT('',#26093);
#6460=VERTEX_POINT('',#26102);
#6461=VERTEX_POINT('',#26104);
#6462=VERTEX_POINT('',#26113);
#6463=VERTEX_POINT('',#26115);
#6464=VERTEX_POINT('',#26124);
#6465=VERTEX_POINT('',#26126);
#6466=VERTEX_POINT('',#26135);
#6467=VERTEX_POINT('',#26137);
#6468=VERTEX_POINT('',#26146);
#6469=VERTEX_POINT('',#26148);
#6470=VERTEX_POINT('',#26157);
#6471=VERTEX_POINT('',#26159);
#6472=VERTEX_POINT('',#26168);
#6473=VERTEX_POINT('',#26170);
#6474=VERTEX_POINT('',#26179);
#6475=VERTEX_POINT('',#26181);
#6476=VERTEX_POINT('',#26190);
#6477=VERTEX_POINT('',#26196);
#6478=VERTEX_POINT('',#26200);
#6479=VERTEX_POINT('',#26203);
#6480=VERTEX_POINT('',#26209);
#6481=VERTEX_POINT('',#26210);
#6482=VERTEX_POINT('',#26213);
#6483=VERTEX_POINT('',#26217);
#6484=VERTEX_POINT('',#26221);
#6485=VERTEX_POINT('',#26224);
#6486=VERTEX_POINT('',#26225);
#6487=VERTEX_POINT('',#26229);
#6488=VERTEX_POINT('',#26231);
#6489=VERTEX_POINT('',#26235);
#6490=VERTEX_POINT('',#26237);
#6491=VERTEX_POINT('',#26239);
#6492=VERTEX_POINT('',#26244);
#6493=VERTEX_POINT('',#26246);
#6494=VERTEX_POINT('',#26248);
#6495=VERTEX_POINT('',#26250);
#6496=VERTEX_POINT('',#26255);
#6497=VERTEX_POINT('',#26257);
#6498=VERTEX_POINT('',#26259);
#6499=VERTEX_POINT('',#26261);
#6500=VERTEX_POINT('',#26263);
#6501=VERTEX_POINT('',#26265);
#6502=VERTEX_POINT('',#26267);
#6503=VERTEX_POINT('',#26269);
#6504=VERTEX_POINT('',#26271);
#6505=VERTEX_POINT('',#26273);
#6506=VERTEX_POINT('',#26275);
#6507=VERTEX_POINT('',#26277);
#6508=VERTEX_POINT('',#26279);
#6509=VERTEX_POINT('',#26281);
#6510=VERTEX_POINT('',#26283);
#6511=VERTEX_POINT('',#26285);
#6512=VERTEX_POINT('',#26287);
#6513=VERTEX_POINT('',#26289);
#6514=VERTEX_POINT('',#26291);
#6515=VERTEX_POINT('',#26293);
#6516=VERTEX_POINT('',#26295);
#6517=VERTEX_POINT('',#26297);
#6518=VERTEX_POINT('',#26299);
#6519=VERTEX_POINT('',#26301);
#6520=VERTEX_POINT('',#26303);
#6521=VERTEX_POINT('',#26305);
#6522=VERTEX_POINT('',#26307);
#6523=VERTEX_POINT('',#26309);
#6524=VERTEX_POINT('',#26312);
#6525=VERTEX_POINT('',#26314);
#6526=VERTEX_POINT('',#26316);
#6527=VERTEX_POINT('',#26318);
#6528=VERTEX_POINT('',#26320);
#6529=VERTEX_POINT('',#26322);
#6530=VERTEX_POINT('',#26324);
#6531=VERTEX_POINT('',#26326);
#6532=VERTEX_POINT('',#26328);
#6533=VERTEX_POINT('',#26330);
#6534=VERTEX_POINT('',#26332);
#6535=VERTEX_POINT('',#26334);
#6536=VERTEX_POINT('',#26336);
#6537=VERTEX_POINT('',#26338);
#6538=VERTEX_POINT('',#26340);
#6539=VERTEX_POINT('',#26342);
#6540=VERTEX_POINT('',#26344);
#6541=VERTEX_POINT('',#26346);
#6542=VERTEX_POINT('',#26348);
#6543=VERTEX_POINT('',#26350);
#6544=VERTEX_POINT('',#26352);
#6545=VERTEX_POINT('',#26354);
#6546=VERTEX_POINT('',#26356);
#6547=VERTEX_POINT('',#26358);
#6548=VERTEX_POINT('',#26360);
#6549=VERTEX_POINT('',#26362);
#6550=VERTEX_POINT('',#26364);
#6551=VERTEX_POINT('',#26366);
#6552=VERTEX_POINT('',#26368);
#6553=VERTEX_POINT('',#26370);
#6554=VERTEX_POINT('',#26372);
#6555=VERTEX_POINT('',#26376);
#6556=VERTEX_POINT('',#26378);
#6557=VERTEX_POINT('',#26388);
#6558=VERTEX_POINT('',#26392);
#6559=VERTEX_POINT('',#26406);
#6560=VERTEX_POINT('',#26410);
#6561=VERTEX_POINT('',#26424);
#6562=VERTEX_POINT('',#26428);
#6563=VERTEX_POINT('',#26442);
#6564=VERTEX_POINT('',#26446);
#6565=VERTEX_POINT('',#26460);
#6566=VERTEX_POINT('',#26464);
#6567=VERTEX_POINT('',#26478);
#6568=VERTEX_POINT('',#26482);
#6569=VERTEX_POINT('',#26505);
#6570=VERTEX_POINT('',#26519);
#6571=VERTEX_POINT('',#26523);
#6572=VERTEX_POINT('',#26537);
#6573=VERTEX_POINT('',#26541);
#6574=VERTEX_POINT('',#26555);
#6575=VERTEX_POINT('',#26559);
#6576=VERTEX_POINT('',#26573);
#6577=VERTEX_POINT('',#26577);
#6578=VERTEX_POINT('',#26591);
#6579=VERTEX_POINT('',#26595);
#6580=VERTEX_POINT('',#26609);
#6581=VERTEX_POINT('',#26613);
#6582=VERTEX_POINT('',#26627);
#6583=VERTEX_POINT('',#26631);
#6584=VERTEX_POINT('',#26645);
#6585=VERTEX_POINT('',#26656);
#6586=VERTEX_POINT('',#26660);
#6587=VERTEX_POINT('',#26664);
#6588=VERTEX_POINT('',#26668);
#6589=VERTEX_POINT('',#26672);
#6590=VERTEX_POINT('',#26676);
#6591=VERTEX_POINT('',#26680);
#6592=VERTEX_POINT('',#26684);
#6593=VERTEX_POINT('',#26688);
#6594=VERTEX_POINT('',#26692);
#6595=VERTEX_POINT('',#26696);
#6596=VERTEX_POINT('',#26700);
#6597=VERTEX_POINT('',#26704);
#6598=VERTEX_POINT('',#26708);
#6599=VERTEX_POINT('',#26712);
#6600=VERTEX_POINT('',#26716);
#6601=VERTEX_POINT('',#26720);
#6602=VERTEX_POINT('',#26724);
#6603=VERTEX_POINT('',#26728);
#6604=VERTEX_POINT('',#26732);
#6605=VERTEX_POINT('',#26736);
#6606=VERTEX_POINT('',#26740);
#6607=VERTEX_POINT('',#26744);
#6608=VERTEX_POINT('',#26748);
#6609=VERTEX_POINT('',#26752);
#6610=VERTEX_POINT('',#26756);
#6611=VERTEX_POINT('',#26760);
#6612=VERTEX_POINT('',#26764);
#6613=VERTEX_POINT('',#26768);
#6614=VERTEX_POINT('',#26807);
#6615=VERTEX_POINT('',#26808);
#6616=VERTEX_POINT('',#26852);
#6617=VERTEX_POINT('',#26856);
#6618=VERTEX_POINT('',#26862);
#6619=VERTEX_POINT('',#26866);
#6620=VERTEX_POINT('',#26867);
#6621=VERTEX_POINT('',#26869);
#6622=VERTEX_POINT('',#26871);
#6623=VERTEX_POINT('',#26873);
#6624=VERTEX_POINT('',#26875);
#6625=VERTEX_POINT('',#26879);
#6626=VERTEX_POINT('',#26880);
#6627=VERTEX_POINT('',#26882);
#6628=VERTEX_POINT('',#26884);
#6629=VERTEX_POINT('',#26888);
#6630=VERTEX_POINT('',#26890);
#6631=VERTEX_POINT('',#26894);
#6632=VERTEX_POINT('',#26895);
#6633=VERTEX_POINT('',#26897);
#6634=VERTEX_POINT('',#26899);
#6635=VERTEX_POINT('',#26903);
#6636=VERTEX_POINT('',#26905);
#6637=VERTEX_POINT('',#26922);
#6638=VERTEX_POINT('',#26979);
#6639=VERTEX_POINT('',#26980);
#6640=VERTEX_POINT('',#26982);
#6641=VERTEX_POINT('',#26993);
#6642=VERTEX_POINT('',#27003);
#6643=VERTEX_POINT('',#27004);
#6644=VERTEX_POINT('',#27051);
#6645=VERTEX_POINT('',#27052);
#6646=VERTEX_POINT('',#27099);
#6647=VERTEX_POINT('',#27100);
#6648=VERTEX_POINT('',#27153);
#6649=VERTEX_POINT('',#27154);
#6650=VERTEX_POINT('',#27201);
#6651=VERTEX_POINT('',#27202);
#6652=VERTEX_POINT('',#27249);
#6653=VERTEX_POINT('',#27250);
#6654=VERTEX_POINT('',#27297);
#6655=VERTEX_POINT('',#27298);
#6656=VERTEX_POINT('',#27351);
#6657=VERTEX_POINT('',#27352);
#6658=VERTEX_POINT('',#27399);
#6659=VERTEX_POINT('',#27400);
#6660=VERTEX_POINT('',#27447);
#6661=VERTEX_POINT('',#27448);
#6662=VERTEX_POINT('',#27501);
#6663=VERTEX_POINT('',#27502);
#6664=VERTEX_POINT('',#27549);
#6665=VERTEX_POINT('',#27550);
#6666=VERTEX_POINT('',#27597);
#6667=VERTEX_POINT('',#27598);
#6668=VERTEX_POINT('',#27651);
#6669=VERTEX_POINT('',#27652);
#6670=VERTEX_POINT('',#27699);
#6671=VERTEX_POINT('',#27700);
#6672=VERTEX_POINT('',#27747);
#6673=VERTEX_POINT('',#27748);
#6674=VERTEX_POINT('',#27795);
#6675=VERTEX_POINT('',#27796);
#6676=VERTEX_POINT('',#27846);
#6677=VERTEX_POINT('',#27847);
#6678=VERTEX_POINT('',#27894);
#6679=VERTEX_POINT('',#27895);
#6680=VERTEX_POINT('',#27942);
#6681=VERTEX_POINT('',#27943);
#6682=VERTEX_POINT('',#27996);
#6683=VERTEX_POINT('',#27997);
#6684=VERTEX_POINT('',#28044);
#6685=VERTEX_POINT('',#28045);
#6686=VERTEX_POINT('',#28092);
#6687=VERTEX_POINT('',#28093);
#6688=VERTEX_POINT('',#28095);
#6689=VERTEX_POINT('',#28104);
#6690=VERTEX_POINT('',#28114);
#6691=VERTEX_POINT('',#28115);
#6692=VERTEX_POINT('',#28138);
#6693=VERTEX_POINT('',#28139);
#6694=VERTEX_POINT('',#28163);
#6695=VERTEX_POINT('',#28164);
#6696=VERTEX_POINT('',#28188);
#6697=VERTEX_POINT('',#28189);
#6698=VERTEX_POINT('',#28212);
#6699=VERTEX_POINT('',#28213);
#6700=VERTEX_POINT('',#28237);
#6701=VERTEX_POINT('',#28238);
#6702=VERTEX_POINT('',#28262);
#6703=VERTEX_POINT('',#28263);
#6704=VERTEX_POINT('',#28286);
#6705=VERTEX_POINT('',#28287);
#6706=VERTEX_POINT('',#28310);
#6707=VERTEX_POINT('',#28311);
#6708=VERTEX_POINT('',#28335);
#6709=VERTEX_POINT('',#28336);
#6710=VERTEX_POINT('',#28360);
#6711=VERTEX_POINT('',#28361);
#6712=VERTEX_POINT('',#28384);
#6713=VERTEX_POINT('',#28385);
#6714=VERTEX_POINT('',#28409);
#6715=VERTEX_POINT('',#28410);
#6716=VERTEX_POINT('',#28434);
#6717=VERTEX_POINT('',#28435);
#6718=VERTEX_POINT('',#28458);
#6719=VERTEX_POINT('',#28459);
#6720=VERTEX_POINT('',#28483);
#6721=VERTEX_POINT('',#28484);
#6722=VERTEX_POINT('',#28508);
#6723=VERTEX_POINT('',#28509);
#6724=VERTEX_POINT('',#28532);
#6725=VERTEX_POINT('',#28533);
#6726=VERTEX_POINT('',#28556);
#6727=VERTEX_POINT('',#28557);
#6728=VERTEX_POINT('',#28581);
#6729=VERTEX_POINT('',#28582);
#6730=VERTEX_POINT('',#28606);
#6731=VERTEX_POINT('',#28607);
#6732=VERTEX_POINT('',#29213);
#6733=VERTEX_POINT('',#29306);
#6734=VERTEX_POINT('',#29405);
#6735=VERTEX_POINT('',#29408);
#6736=VERTEX_POINT('',#30088);
#6737=VERTEX_POINT('',#30184);
#6738=VERTEX_POINT('',#30189);
#6739=VERTEX_POINT('',#30190);
#6740=VERTEX_POINT('',#30194);
#6741=VERTEX_POINT('',#30198);
#6742=VERTEX_POINT('',#30202);
#6743=VERTEX_POINT('',#30206);
#6744=VERTEX_POINT('',#30210);
#6745=VERTEX_POINT('',#30213);
#6746=VERTEX_POINT('',#30221);
#6747=VERTEX_POINT('',#30223);
#6748=VERTEX_POINT('',#30227);
#6749=VERTEX_POINT('',#30231);
#6750=VERTEX_POINT('',#30235);
#6751=VERTEX_POINT('',#30239);
#6752=VERTEX_POINT('',#30248);
#6753=VERTEX_POINT('',#30249);
#6754=VERTEX_POINT('',#30251);
#6755=VERTEX_POINT('',#30262);
#6756=VERTEX_POINT('',#30272);
#6757=VERTEX_POINT('',#30273);
#6758=VERTEX_POINT('',#30320);
#6759=VERTEX_POINT('',#30321);
#6760=VERTEX_POINT('',#30368);
#6761=VERTEX_POINT('',#30369);
#6762=VERTEX_POINT('',#30422);
#6763=VERTEX_POINT('',#30423);
#6764=VERTEX_POINT('',#30470);
#6765=VERTEX_POINT('',#30471);
#6766=VERTEX_POINT('',#30518);
#6767=VERTEX_POINT('',#30519);
#6768=VERTEX_POINT('',#30566);
#6769=VERTEX_POINT('',#30567);
#6770=VERTEX_POINT('',#30620);
#6771=VERTEX_POINT('',#30621);
#6772=VERTEX_POINT('',#30668);
#6773=VERTEX_POINT('',#30669);
#6774=VERTEX_POINT('',#30716);
#6775=VERTEX_POINT('',#30717);
#6776=VERTEX_POINT('',#30770);
#6777=VERTEX_POINT('',#30771);
#6778=VERTEX_POINT('',#30818);
#6779=VERTEX_POINT('',#30819);
#6780=VERTEX_POINT('',#30866);
#6781=VERTEX_POINT('',#30867);
#6782=VERTEX_POINT('',#30920);
#6783=VERTEX_POINT('',#30921);
#6784=VERTEX_POINT('',#30968);
#6785=VERTEX_POINT('',#30969);
#6786=VERTEX_POINT('',#31016);
#6787=VERTEX_POINT('',#31017);
#6788=VERTEX_POINT('',#31064);
#6789=VERTEX_POINT('',#31065);
#6790=VERTEX_POINT('',#31118);
#6791=VERTEX_POINT('',#31119);
#6792=VERTEX_POINT('',#31166);
#6793=VERTEX_POINT('',#31167);
#6794=VERTEX_POINT('',#31214);
#6795=VERTEX_POINT('',#31215);
#6796=VERTEX_POINT('',#31268);
#6797=VERTEX_POINT('',#31269);
#6798=VERTEX_POINT('',#31316);
#6799=VERTEX_POINT('',#31317);
#6800=VERTEX_POINT('',#31364);
#6801=VERTEX_POINT('',#31365);
#6802=VERTEX_POINT('',#31418);
#6803=VERTEX_POINT('',#31419);
#6804=VERTEX_POINT('',#31466);
#6805=VERTEX_POINT('',#31467);
#6806=VERTEX_POINT('',#31514);
#6807=VERTEX_POINT('',#31515);
#6808=VERTEX_POINT('',#31568);
#6809=VERTEX_POINT('',#31569);
#6810=VERTEX_POINT('',#31616);
#6811=VERTEX_POINT('',#31617);
#6812=VERTEX_POINT('',#31619);
#6813=VERTEX_POINT('',#31626);
#6814=VERTEX_POINT('',#31634);
#6815=VERTEX_POINT('',#31635);
#6816=VERTEX_POINT('',#31658);
#6817=VERTEX_POINT('',#31659);
#6818=VERTEX_POINT('',#31683);
#6819=VERTEX_POINT('',#31684);
#6820=VERTEX_POINT('',#31708);
#6821=VERTEX_POINT('',#31709);
#6822=VERTEX_POINT('',#31732);
#6823=VERTEX_POINT('',#31733);
#6824=VERTEX_POINT('',#31757);
#6825=VERTEX_POINT('',#31758);
#6826=VERTEX_POINT('',#31782);
#6827=VERTEX_POINT('',#31783);
#6828=VERTEX_POINT('',#31806);
#6829=VERTEX_POINT('',#31807);
#6830=VERTEX_POINT('',#31831);
#6831=VERTEX_POINT('',#31832);
#6832=VERTEX_POINT('',#31856);
#6833=VERTEX_POINT('',#31857);
#6834=VERTEX_POINT('',#31880);
#6835=VERTEX_POINT('',#31881);
#6836=VERTEX_POINT('',#31905);
#6837=VERTEX_POINT('',#31906);
#6838=VERTEX_POINT('',#31930);
#6839=VERTEX_POINT('',#31931);
#6840=VERTEX_POINT('',#31954);
#6841=VERTEX_POINT('',#31955);
#6842=VERTEX_POINT('',#31978);
#6843=VERTEX_POINT('',#31979);
#6844=VERTEX_POINT('',#32003);
#6845=VERTEX_POINT('',#32004);
#6846=VERTEX_POINT('',#32028);
#6847=VERTEX_POINT('',#32029);
#6848=VERTEX_POINT('',#32052);
#6849=VERTEX_POINT('',#32053);
#6850=VERTEX_POINT('',#32077);
#6851=VERTEX_POINT('',#32078);
#6852=VERTEX_POINT('',#32102);
#6853=VERTEX_POINT('',#32103);
#6854=VERTEX_POINT('',#32126);
#6855=VERTEX_POINT('',#32127);
#6856=VERTEX_POINT('',#32151);
#6857=VERTEX_POINT('',#32152);
#6858=VERTEX_POINT('',#32176);
#6859=VERTEX_POINT('',#32177);
#6860=VERTEX_POINT('',#32200);
#6861=VERTEX_POINT('',#32201);
#6862=VERTEX_POINT('',#32224);
#6863=VERTEX_POINT('',#32225);
#6864=VERTEX_POINT('',#32249);
#6865=VERTEX_POINT('',#32250);
#6866=VERTEX_POINT('',#32274);
#6867=VERTEX_POINT('',#32275);
#6868=VERTEX_POINT('',#33025);
#6869=VERTEX_POINT('',#33130);
#6870=VERTEX_POINT('',#33229);
#6871=VERTEX_POINT('',#33232);
#6872=VERTEX_POINT('',#34056);
#6873=VERTEX_POINT('',#34162);
#6874=VERTEX_POINT('',#34163);
#6875=VERTEX_POINT('',#34167);
#6876=VERTEX_POINT('',#34168);
#6877=VERTEX_POINT('',#34175);
#6878=VERTEX_POINT('',#34177);
#6879=VERTEX_POINT('',#34181);
#6880=VERTEX_POINT('',#34188);
#6881=VERTEX_POINT('',#34192);
#6882=VERTEX_POINT('',#34199);
#6883=VERTEX_POINT('',#34203);
#6884=VERTEX_POINT('',#34210);
#6885=VERTEX_POINT('',#34214);
#6886=VERTEX_POINT('',#34221);
#6887=VERTEX_POINT('',#34234);
#6888=VERTEX_POINT('',#34241);
#6889=VERTEX_POINT('',#34244);
#6890=VERTEX_POINT('',#34245);
#6891=VERTEX_POINT('',#34281);
#6892=VERTEX_POINT('',#34283);
#6893=VERTEX_POINT('',#34285);
#6894=VERTEX_POINT('',#34289);
#6895=VERTEX_POINT('',#34293);
#6896=VERTEX_POINT('',#34296);
#6897=VERTEX_POINT('',#34300);
#6898=VERTEX_POINT('',#34306);
#6899=VERTEX_POINT('',#34307);
#6900=VERTEX_POINT('',#34311);
#6901=VERTEX_POINT('',#34313);
#6902=VERTEX_POINT('',#34319);
#6903=VERTEX_POINT('',#34323);
#6904=VERTEX_POINT('',#34329);
#6905=VERTEX_POINT('',#34333);
#6906=VERTEX_POINT('',#34337);
#6907=VERTEX_POINT('',#34341);
#6908=VERTEX_POINT('',#34345);
#6909=VERTEX_POINT('',#34349);
#6910=VERTEX_POINT('',#34352);
#6911=VERTEX_POINT('',#34356);
#6912=VERTEX_POINT('',#34360);
#6913=VERTEX_POINT('',#34364);
#6914=VERTEX_POINT('',#34368);
#6915=VERTEX_POINT('',#34376);
#6916=VERTEX_POINT('',#34378);
#6917=VERTEX_POINT('',#34382);
#6918=VERTEX_POINT('',#34386);
#6919=VERTEX_POINT('',#34389);
#6920=VERTEX_POINT('',#34394);
#6921=VERTEX_POINT('',#34396);
#6922=VERTEX_POINT('',#34402);
#6923=VERTEX_POINT('',#34408);
#6924=VERTEX_POINT('',#34410);
#6925=VERTEX_POINT('',#34420);
#6926=VERTEX_POINT('',#34424);
#6927=VERTEX_POINT('',#34428);
#6928=VERTEX_POINT('',#34432);
#6929=VERTEX_POINT('',#34436);
#6930=VERTEX_POINT('',#34459);
#6931=VERTEX_POINT('',#34460);
#6932=VERTEX_POINT('',#34462);
#6933=VERTEX_POINT('',#34473);
#6934=VERTEX_POINT('',#34483);
#6935=VERTEX_POINT('',#34484);
#6936=VERTEX_POINT('',#34531);
#6937=VERTEX_POINT('',#34532);
#6938=VERTEX_POINT('',#34579);
#6939=VERTEX_POINT('',#34580);
#6940=VERTEX_POINT('',#34630);
#6941=VERTEX_POINT('',#34631);
#6942=VERTEX_POINT('',#34681);
#6943=VERTEX_POINT('',#34682);
#6944=VERTEX_POINT('',#34729);
#6945=VERTEX_POINT('',#34730);
#6946=VERTEX_POINT('',#34777);
#6947=VERTEX_POINT('',#34778);
#6948=VERTEX_POINT('',#34831);
#6949=VERTEX_POINT('',#34832);
#6950=VERTEX_POINT('',#34879);
#6951=VERTEX_POINT('',#34880);
#6952=VERTEX_POINT('',#34927);
#6953=VERTEX_POINT('',#34928);
#6954=VERTEX_POINT('',#34981);
#6955=VERTEX_POINT('',#34982);
#6956=VERTEX_POINT('',#35029);
#6957=VERTEX_POINT('',#35030);
#6958=VERTEX_POINT('',#35077);
#6959=VERTEX_POINT('',#35078);
#6960=VERTEX_POINT('',#35125);
#6961=VERTEX_POINT('',#35126);
#6962=VERTEX_POINT('',#35179);
#6963=VERTEX_POINT('',#35180);
#6964=VERTEX_POINT('',#35227);
#6965=VERTEX_POINT('',#35228);
#6966=VERTEX_POINT('',#35275);
#6967=VERTEX_POINT('',#35276);
#6968=VERTEX_POINT('',#35278);
#6969=VERTEX_POINT('',#35328);
#6970=VERTEX_POINT('',#35329);
#6971=VERTEX_POINT('',#35331);
#6972=VERTEX_POINT('',#35340);
#6973=VERTEX_POINT('',#35349);
#6974=VERTEX_POINT('',#35350);
#6975=VERTEX_POINT('',#35374);
#6976=VERTEX_POINT('',#35375);
#6977=VERTEX_POINT('',#35398);
#6978=VERTEX_POINT('',#35399);
#6979=VERTEX_POINT('',#35423);
#6980=VERTEX_POINT('',#35424);
#6981=VERTEX_POINT('',#35448);
#6982=VERTEX_POINT('',#35449);
#6983=VERTEX_POINT('',#35472);
#6984=VERTEX_POINT('',#35473);
#6985=VERTEX_POINT('',#35496);
#6986=VERTEX_POINT('',#35497);
#6987=VERTEX_POINT('',#35521);
#6988=VERTEX_POINT('',#35522);
#6989=VERTEX_POINT('',#35546);
#6990=VERTEX_POINT('',#35547);
#6991=VERTEX_POINT('',#35570);
#6992=VERTEX_POINT('',#35571);
#6993=VERTEX_POINT('',#35595);
#6994=VERTEX_POINT('',#35596);
#6995=VERTEX_POINT('',#35620);
#6996=VERTEX_POINT('',#35621);
#6997=VERTEX_POINT('',#35644);
#6998=VERTEX_POINT('',#35645);
#6999=VERTEX_POINT('',#35669);
#7000=VERTEX_POINT('',#35670);
#7001=VERTEX_POINT('',#35693);
#7002=VERTEX_POINT('',#35694);
#7003=VERTEX_POINT('',#35718);
#7004=VERTEX_POINT('',#35719);
#7005=VERTEX_POINT('',#36197);
#7006=VERTEX_POINT('',#36284);
#7007=VERTEX_POINT('',#36377);
#7008=VERTEX_POINT('',#36380);
#7009=VERTEX_POINT('',#37012);
#7010=VERTEX_POINT('',#37013);
#7011=VERTEX_POINT('',#37017);
#7012=VERTEX_POINT('',#37018);
#7013=VERTEX_POINT('',#37025);
#7014=VERTEX_POINT('',#37027);
#7015=VERTEX_POINT('',#37031);
#7016=VERTEX_POINT('',#37038);
#7017=VERTEX_POINT('',#37042);
#7018=VERTEX_POINT('',#37049);
#7019=VERTEX_POINT('',#37053);
#7020=VERTEX_POINT('',#37060);
#7021=VERTEX_POINT('',#37064);
#7022=VERTEX_POINT('',#37071);
#7023=VERTEX_POINT('',#37084);
#7024=VERTEX_POINT('',#37091);
#7025=VERTEX_POINT('',#37094);
#7026=VERTEX_POINT('',#37095);
#7027=EDGE_CURVE('',#5681,#5682,#3203,.T.);
#7028=EDGE_CURVE('',#5682,#5683,#3204,.T.);
#7029=EDGE_CURVE('',#5683,#5684,#3205,.T.);
#7030=EDGE_CURVE('',#5684,#5685,#3098,.T.);
#7031=EDGE_CURVE('',#5685,#5686,#3206,.T.);
#7032=EDGE_CURVE('',#5686,#5681,#3099,.T.);
#7033=EDGE_CURVE('',#5681,#5687,#3100,.T.);
#7034=EDGE_CURVE('',#5687,#5688,#3207,.T.);
#7035=EDGE_CURVE('',#5688,#5689,#3208,.T.);
#7036=EDGE_CURVE('',#5689,#5682,#3209,.T.);
#7037=EDGE_CURVE('',#5686,#5690,#951,.T.);
#7038=EDGE_CURVE('',#5691,#5690,#3101,.T.);
#7039=EDGE_CURVE('',#5692,#5691,#3102,.T.);
#7040=EDGE_CURVE('',#5692,#5687,#952,.T.);
#7041=EDGE_CURVE('',#5693,#5685,#953,.T.);
#7042=EDGE_CURVE('',#5690,#5693,#3210,.T.);
#7043=EDGE_CURVE('',#5694,#5688,#3211,.T.);
#7044=EDGE_CURVE('',#5689,#5694,#3212,.T.);
#7045=EDGE_CURVE('',#5695,#5696,#3213,.T.);
#7046=EDGE_CURVE('',#5697,#5695,#3214,.T.);
#7047=EDGE_CURVE('',#5696,#5697,#3215,.T.);
#7048=EDGE_CURVE('',#5698,#5699,#3216,.T.);
#7049=EDGE_CURVE('',#5699,#5697,#3217,.T.);
#7050=EDGE_CURVE('',#5695,#5698,#3218,.T.);
#7051=EDGE_CURVE('',#5698,#5700,#954,.T.);
#7052=EDGE_CURVE('',#5700,#5701,#3219,.T.);
#7053=EDGE_CURVE('',#5701,#5699,#955,.T.);
#7054=EDGE_CURVE('',#5702,#5703,#3103,.F.);
#7055=EDGE_CURVE('',#5703,#5701,#3220,.T.);
#7056=EDGE_CURVE('',#5700,#5702,#3221,.T.);
#7057=EDGE_CURVE('',#5683,#5696,#3222,.T.);
#7058=EDGE_CURVE('',#5697,#5704,#3223,.T.);
#7059=EDGE_CURVE('',#5704,#5684,#3104,.T.);
#7060=EDGE_CURVE('',#5694,#5695,#3224,.T.);
#7061=EDGE_CURVE('',#5696,#5689,#3225,.T.);
#7062=EDGE_CURVE('',#5705,#5706,#3105,.F.);
#7063=EDGE_CURVE('',#5706,#5707,#3226,.T.);
#7064=EDGE_CURVE('',#5707,#5708,#3227,.T.);
#7065=EDGE_CURVE('',#5708,#5705,#3228,.T.);
#7066=EDGE_CURVE('',#5707,#5709,#956,.T.);
#7067=EDGE_CURVE('',#5709,#5710,#3229,.T.);
#7068=EDGE_CURVE('',#5710,#5708,#957,.T.);
#7069=EDGE_CURVE('',#5709,#5694,#3230,.T.);
#7070=EDGE_CURVE('',#5688,#5710,#3231,.T.);
#7071=EDGE_CURVE('',#5711,#5703,#958,.T.);
#7072=EDGE_CURVE('',#5712,#5711,#3232,.T.);
#7073=EDGE_CURVE('',#5713,#5712,#959,.T.);
#7074=EDGE_CURVE('',#5714,#5713,#3233,.T.);
#7075=EDGE_CURVE('',#5715,#5714,#3234,.T.);
#7076=EDGE_CURVE('',#5704,#5715,#960,.T.);
#7077=EDGE_CURVE('',#5698,#5709,#3235,.T.);
#7078=EDGE_CURVE('',#5707,#5700,#3236,.T.);
#7079=EDGE_CURVE('',#5716,#5706,#3106,.F.);
#7080=EDGE_CURVE('',#5717,#5716,#3237,.T.);
#7081=EDGE_CURVE('',#5702,#5717,#3107,.F.);
#7082=EDGE_CURVE('',#5718,#5718,#961,.T.);
#7083=EDGE_CURVE('',#5719,#5720,#3238,.T.);
#7084=EDGE_CURVE('',#5720,#5721,#3239,.T.);
#7085=EDGE_CURVE('',#5721,#5691,#3240,.T.);
#7086=EDGE_CURVE('',#5693,#5719,#3108,.T.);
#7087=EDGE_CURVE('',#5721,#5722,#3241,.T.);
#7088=EDGE_CURVE('',#5722,#5723,#3242,.T.);
#7089=EDGE_CURVE('',#5723,#5692,#3243,.T.);
#7090=EDGE_CURVE('',#5724,#5722,#3244,.T.);
#7091=EDGE_CURVE('',#5723,#5724,#3245,.T.);
#7092=EDGE_CURVE('',#5725,#5726,#3246,.T.);
#7093=EDGE_CURVE('',#5714,#5725,#3247,.T.);
#7094=EDGE_CURVE('',#5726,#5714,#3248,.T.);
#7095=EDGE_CURVE('',#5719,#5715,#3109,.T.);
#7096=EDGE_CURVE('',#5725,#5720,#3249,.T.);
#7097=EDGE_CURVE('',#5711,#5727,#3110,.F.);
#7098=EDGE_CURVE('',#5727,#5728,#3250,.T.);
#7099=EDGE_CURVE('',#5728,#5712,#3251,.T.);
#7100=EDGE_CURVE('',#5728,#5729,#962,.T.);
#7101=EDGE_CURVE('',#5729,#5713,#3252,.T.);
#7102=EDGE_CURVE('',#5729,#5726,#3253,.T.);
#7103=EDGE_CURVE('',#5722,#5725,#3254,.T.);
#7104=EDGE_CURVE('',#5726,#5724,#3255,.T.);
#7105=EDGE_CURVE('',#5730,#5731,#3256,.T.);
#7106=EDGE_CURVE('',#5731,#5723,#3257,.T.);
#7107=EDGE_CURVE('',#5724,#5730,#3258,.T.);
#7108=EDGE_CURVE('',#5730,#5732,#963,.T.);
#7109=EDGE_CURVE('',#5732,#5733,#3259,.T.);
#7110=EDGE_CURVE('',#5733,#5731,#964,.T.);
#7111=EDGE_CURVE('',#5734,#5735,#3111,.F.);
#7112=EDGE_CURVE('',#5735,#5733,#3260,.T.);
#7113=EDGE_CURVE('',#5732,#5734,#3261,.T.);
#7114=EDGE_CURVE('',#5736,#5736,#965,.T.);
#7115=EDGE_CURVE('',#5737,#5727,#3112,.F.);
#7116=EDGE_CURVE('',#5717,#5737,#966,.T.);
#7117=EDGE_CURVE('',#5734,#5738,#3113,.F.);
#7118=EDGE_CURVE('',#5738,#5716,#967,.T.);
#7119=EDGE_CURVE('',#5705,#5735,#968,.T.);
#7120=EDGE_CURVE('',#5737,#5738,#3262,.T.);
#7121=EDGE_CURVE('',#5718,#5739,#3263,.T.);
#7122=EDGE_CURVE('',#5739,#5739,#969,.T.);
#7123=EDGE_CURVE('',#5740,#5740,#970,.T.);
#7124=EDGE_CURVE('',#5740,#5736,#3264,.T.);
#7125=EDGE_CURVE('',#5728,#5732,#3265,.T.);
#7126=EDGE_CURVE('',#5730,#5729,#3266,.T.);
#7127=EDGE_CURVE('',#5741,#5742,#3267,.F.);
#7128=EDGE_CURVE('',#5742,#5743,#3268,.T.);
#7129=EDGE_CURVE('',#5743,#5744,#3269,.T.);
#7130=EDGE_CURVE('',#5744,#5741,#3270,.T.);
#7131=EDGE_CURVE('',#5743,#5745,#971,.T.);
#7132=EDGE_CURVE('',#5745,#5746,#3271,.T.);
#7133=EDGE_CURVE('',#5746,#5744,#972,.T.);
#7134=EDGE_CURVE('',#5747,#5748,#3272,.T.);
#7135=EDGE_CURVE('',#5748,#5746,#3273,.T.);
#7136=EDGE_CURVE('',#5745,#5747,#3274,.T.);
#7137=EDGE_CURVE('',#5747,#5749,#973,.T.);
#7138=EDGE_CURVE('',#5749,#5750,#3275,.T.);
#7139=EDGE_CURVE('',#5750,#5748,#974,.T.);
#7140=EDGE_CURVE('',#5751,#5750,#3276,.T.);
#7141=EDGE_CURVE('',#5749,#5752,#3277,.T.);
#7142=EDGE_CURVE('',#5752,#5751,#3278,.T.);
#7143=EDGE_CURVE('',#5752,#5753,#3279,.T.);
#7144=EDGE_CURVE('',#5753,#5754,#3114,.F.);
#7145=EDGE_CURVE('',#5754,#5751,#3280,.T.);
#7146=EDGE_CURVE('',#5741,#5751,#3281,.T.);
#7147=EDGE_CURVE('',#5755,#5755,#975,.T.);
#7148=EDGE_CURVE('',#5756,#5754,#3115,.F.);
#7149=EDGE_CURVE('',#5757,#5756,#3282,.T.);
#7150=EDGE_CURVE('',#5758,#5757,#3116,.F.);
#7151=EDGE_CURVE('',#5741,#5758,#3283,.T.);
#7152=EDGE_CURVE('',#5759,#5760,#3284,.T.);
#7153=EDGE_CURVE('',#5760,#5761,#3285,.T.);
#7154=EDGE_CURVE('',#5761,#5762,#3286,.T.);
#7155=EDGE_CURVE('',#5762,#5759,#3287,.T.);
#7156=EDGE_CURVE('',#5763,#5764,#3288,.T.);
#7157=EDGE_CURVE('',#5764,#5765,#3289,.T.);
#7158=EDGE_CURVE('',#5765,#5766,#3290,.T.);
#7159=EDGE_CURVE('',#5766,#5763,#3291,.T.);
#7160=EDGE_CURVE('',#5766,#5767,#3292,.T.);
#7161=EDGE_CURVE('',#5767,#5768,#3293,.T.);
#7162=EDGE_CURVE('',#5768,#5763,#3294,.T.);
#7163=EDGE_CURVE('',#5769,#5770,#3295,.T.);
#7164=EDGE_CURVE('',#5770,#5768,#976,.T.);
#7165=EDGE_CURVE('',#5767,#5769,#977,.T.);
#7166=EDGE_CURVE('',#5771,#5772,#3296,.T.);
#7167=EDGE_CURVE('',#5772,#5770,#3297,.T.);
#7168=EDGE_CURVE('',#5769,#5773,#3298,.T.);
#7169=EDGE_CURVE('',#5773,#5771,#3299,.T.);
#7170=EDGE_CURVE('',#5774,#5775,#3300,.T.);
#7171=EDGE_CURVE('',#5775,#5765,#978,.T.);
#7172=EDGE_CURVE('',#5764,#5774,#979,.T.);
#7173=EDGE_CURVE('',#5776,#5777,#3301,.T.);
#7174=EDGE_CURVE('',#5777,#5775,#3302,.T.);
#7175=EDGE_CURVE('',#5774,#5776,#3303,.T.);
#7176=EDGE_CURVE('',#5778,#5779,#3304,.T.);
#7177=EDGE_CURVE('',#5779,#5777,#980,.T.);
#7178=EDGE_CURVE('',#5776,#5778,#981,.T.);
#7179=EDGE_CURVE('',#5762,#5779,#3305,.T.);
#7180=EDGE_CURVE('',#5778,#5759,#3306,.T.);
#7181=EDGE_CURVE('',#5760,#5780,#982,.T.);
#7182=EDGE_CURVE('',#5780,#5781,#3307,.T.);
#7183=EDGE_CURVE('',#5781,#5761,#983,.T.);
#7184=EDGE_CURVE('',#5782,#5783,#3308,.T.);
#7185=EDGE_CURVE('',#5783,#5781,#3309,.T.);
#7186=EDGE_CURVE('',#5780,#5784,#3310,.T.);
#7187=EDGE_CURVE('',#5784,#5782,#3311,.T.);
#7188=EDGE_CURVE('',#5785,#5742,#3312,.T.);
#7189=EDGE_CURVE('',#5786,#5785,#984,.T.);
#7190=EDGE_CURVE('',#5787,#5786,#3313,.T.);
#7191=EDGE_CURVE('',#5788,#5787,#3314,.T.);
#7192=EDGE_CURVE('',#5789,#5788,#3315,.T.);
#7193=EDGE_CURVE('',#5790,#5789,#3316,.T.);
#7194=EDGE_CURVE('',#5791,#5790,#3317,.T.);
#7195=EDGE_CURVE('',#5792,#5791,#985,.T.);
#7196=EDGE_CURVE('',#5793,#5792,#3318,.T.);
#7197=EDGE_CURVE('',#5794,#5793,#3319,.T.);
#7198=EDGE_CURVE('',#5795,#5794,#986,.T.);
#7199=EDGE_CURVE('',#5773,#5795,#3320,.T.);
#7200=EDGE_CURVE('',#5743,#5765,#3321,.T.);
#7201=EDGE_CURVE('',#5775,#5745,#3322,.T.);
#7202=EDGE_CURVE('',#5747,#5777,#3323,.T.);
#7203=EDGE_CURVE('',#5779,#5749,#3324,.T.);
#7204=EDGE_CURVE('',#5796,#5783,#3325,.T.);
#7205=EDGE_CURVE('',#5797,#5796,#987,.T.);
#7206=EDGE_CURVE('',#5798,#5797,#3326,.T.);
#7207=EDGE_CURVE('',#5799,#5798,#3327,.T.);
#7208=EDGE_CURVE('',#5800,#5799,#988,.T.);
#7209=EDGE_CURVE('',#5801,#5800,#3328,.T.);
#7210=EDGE_CURVE('',#5802,#5801,#3329,.T.);
#7211=EDGE_CURVE('',#5803,#5802,#3330,.T.);
#7212=EDGE_CURVE('',#5804,#5803,#3331,.T.);
#7213=EDGE_CURVE('',#5805,#5804,#3332,.T.);
#7214=EDGE_CURVE('',#5753,#5805,#989,.T.);
#7215=EDGE_CURVE('',#5806,#5782,#3333,.T.);
#7216=EDGE_CURVE('',#5806,#5807,#3334,.T.);
#7217=EDGE_CURVE('',#5807,#5808,#3335,.T.);
#7218=EDGE_CURVE('',#5808,#5796,#3117,.T.);
#7219=EDGE_CURVE('',#5804,#5809,#3336,.F.);
#7220=EDGE_CURVE('',#5809,#5810,#3337,.T.);
#7221=EDGE_CURVE('',#5810,#5805,#3118,.F.);
#7222=EDGE_CURVE('',#5811,#5809,#3338,.T.);
#7223=EDGE_CURVE('',#5812,#5811,#3339,.T.);
#7224=EDGE_CURVE('',#5813,#5812,#3119,.F.);
#7225=EDGE_CURVE('',#5813,#5814,#3340,.T.);
#7226=EDGE_CURVE('',#5810,#5814,#3120,.F.);
#7227=EDGE_CURVE('',#5815,#5798,#3341,.T.);
#7228=EDGE_CURVE('',#5816,#5815,#3342,.T.);
#7229=EDGE_CURVE('',#5798,#5816,#3343,.T.);
#7230=EDGE_CURVE('',#5817,#5818,#3344,.T.);
#7231=EDGE_CURVE('',#5818,#5816,#3345,.T.);
#7232=EDGE_CURVE('',#5815,#5819,#3346,.T.);
#7233=EDGE_CURVE('',#5819,#5817,#3347,.T.);
#7234=EDGE_CURVE('',#5820,#5799,#3348,.T.);
#7235=EDGE_CURVE('',#5816,#5820,#3349,.T.);
#7236=EDGE_CURVE('',#5820,#5821,#990,.T.);
#7237=EDGE_CURVE('',#5821,#5800,#3350,.T.);
#7238=EDGE_CURVE('',#5822,#5801,#3351,.F.);
#7239=EDGE_CURVE('',#5821,#5822,#3352,.T.);
#7240=EDGE_CURVE('',#5823,#5824,#3353,.T.);
#7241=EDGE_CURVE('',#5824,#5815,#3354,.T.);
#7242=EDGE_CURVE('',#5797,#5823,#3121,.T.);
#7243=EDGE_CURVE('',#5820,#5825,#3355,.T.);
#7244=EDGE_CURVE('',#5826,#5825,#991,.T.);
#7245=EDGE_CURVE('',#5826,#5821,#3356,.T.);
#7246=EDGE_CURVE('',#5825,#5818,#3357,.T.);
#7247=EDGE_CURVE('',#5793,#5817,#3358,.T.);
#7248=EDGE_CURVE('',#5792,#5825,#3359,.T.);
#7249=EDGE_CURVE('',#5819,#5827,#3360,.T.);
#7250=EDGE_CURVE('',#5827,#5828,#3361,.T.);
#7251=EDGE_CURVE('',#5828,#5794,#3122,.T.);
#7252=EDGE_CURVE('',#5827,#5824,#3362,.T.);
#7253=EDGE_CURVE('',#5829,#5829,#992,.T.);
#7254=EDGE_CURVE('',#5823,#5830,#3123,.T.);
#7255=EDGE_CURVE('',#5830,#5831,#3363,.T.);
#7256=EDGE_CURVE('',#5831,#5828,#3124,.T.);
#7257=EDGE_CURVE('',#5791,#5826,#3364,.T.);
#7258=EDGE_CURVE('',#5832,#5826,#3365,.T.);
#7259=EDGE_CURVE('',#5790,#5832,#3366,.T.);
#7260=EDGE_CURVE('',#5822,#5833,#3367,.T.);
#7261=EDGE_CURVE('',#5833,#5802,#3368,.T.);
#7262=EDGE_CURVE('',#5834,#5835,#3369,.T.);
#7263=EDGE_CURVE('',#5835,#5802,#993,.T.);
#7264=EDGE_CURVE('',#5833,#5834,#994,.T.);
#7265=EDGE_CURVE('',#5834,#5836,#3370,.T.);
#7266=EDGE_CURVE('',#5836,#5837,#3371,.T.);
#7267=EDGE_CURVE('',#5837,#5835,#3372,.T.);
#7268=EDGE_CURVE('',#5838,#5789,#3373,.T.);
#7269=EDGE_CURVE('',#5789,#5837,#995,.T.);
#7270=EDGE_CURVE('',#5836,#5838,#996,.T.);
#7271=EDGE_CURVE('',#5838,#5832,#3374,.T.);
#7272=EDGE_CURVE('',#5832,#5822,#3375,.T.);
#7273=EDGE_CURVE('',#5839,#5839,#997,.T.);
#7274=EDGE_CURVE('',#5840,#5840,#998,.T.);
#7275=EDGE_CURVE('',#5811,#5841,#3376,.T.);
#7276=EDGE_CURVE('',#5841,#5788,#3377,.T.);
#7277=EDGE_CURVE('',#5787,#5811,#3378,.T.);
#7278=EDGE_CURVE('',#5786,#5812,#3125,.F.);
#7279=EDGE_CURVE('',#5842,#5843,#3379,.T.);
#7280=EDGE_CURVE('',#5843,#5788,#999,.T.);
#7281=EDGE_CURVE('',#5841,#5842,#1000,.T.);
#7282=EDGE_CURVE('',#5844,#5845,#3380,.T.);
#7283=EDGE_CURVE('',#5845,#5843,#3381,.T.);
#7284=EDGE_CURVE('',#5842,#5844,#3382,.T.);
#7285=EDGE_CURVE('',#5846,#5803,#3383,.T.);
#7286=EDGE_CURVE('',#5803,#5845,#1001,.T.);
#7287=EDGE_CURVE('',#5844,#5846,#1002,.T.);
#7288=EDGE_CURVE('',#5846,#5809,#3384,.T.);
#7289=EDGE_CURVE('',#5847,#5847,#1003,.T.);
#7290=EDGE_CURVE('',#5758,#5785,#3126,.F.);
#7291=EDGE_CURVE('',#5795,#5848,#3127,.T.);
#7292=EDGE_CURVE('',#5848,#5849,#3385,.T.);
#7293=EDGE_CURVE('',#5849,#5850,#3386,.T.);
#7294=EDGE_CURVE('',#5850,#5771,#3387,.T.);
#7295=EDGE_CURVE('',#5850,#5806,#3388,.T.);
#7296=EDGE_CURVE('',#5784,#5772,#3389,.T.);
#7297=EDGE_CURVE('',#5831,#5851,#1004,.T.);
#7298=EDGE_CURVE('',#5848,#5851,#3128,.T.);
#7299=EDGE_CURVE('',#5770,#5780,#3390,.T.);
#7300=EDGE_CURVE('',#5852,#5808,#3129,.T.);
#7301=EDGE_CURVE('',#5852,#5830,#1005,.T.);
#7302=EDGE_CURVE('',#5851,#5852,#3391,.T.);
#7303=EDGE_CURVE('',#5853,#5854,#3392,.T.);
#7304=EDGE_CURVE('',#5855,#5853,#1006,.T.);
#7305=EDGE_CURVE('',#5856,#5855,#3393,.T.);
#7306=EDGE_CURVE('',#5854,#5856,#1007,.T.);
#7307=EDGE_CURVE('',#5807,#5849,#3394,.T.);
#7308=EDGE_CURVE('',#5855,#5857,#120,.T.);
#7309=EDGE_CURVE('',#5857,#5858,#3395,.T.);
#7310=EDGE_CURVE('',#5858,#5856,#121,.T.);
#7311=EDGE_CURVE('',#5854,#5859,#122,.T.);
#7312=EDGE_CURVE('',#5859,#5860,#3396,.T.);
#7313=EDGE_CURVE('',#5860,#5853,#123,.T.);
#7314=EDGE_CURVE('',#5861,#5862,#1008,.T.);
#7315=EDGE_CURVE('',#5862,#5859,#3130,.T.);
#7316=EDGE_CURVE('',#5858,#5861,#3131,.T.);
#7317=EDGE_CURVE('',#5860,#5863,#3132,.T.);
#7318=EDGE_CURVE('',#5863,#5864,#1009,.T.);
#7319=EDGE_CURVE('',#5864,#5857,#3133,.T.);
#7320=EDGE_CURVE('',#5865,#5863,#3397,.T.);
#7321=EDGE_CURVE('',#5866,#5865,#3398,.T.);
#7322=EDGE_CURVE('',#5867,#5866,#1010,.T.);
#7323=EDGE_CURVE('',#5868,#5867,#3399,.T.);
#7324=EDGE_CURVE('',#5864,#5868,#3400,.T.);
#7325=EDGE_CURVE('',#5862,#5869,#3401,.T.);
#7326=EDGE_CURVE('',#5865,#5869,#3402,.T.);
#7327=EDGE_CURVE('',#5870,#5871,#3403,.T.);
#7328=EDGE_CURVE('',#5871,#5872,#124,.T.);
#7329=EDGE_CURVE('',#5872,#5873,#3404,.T.);
#7330=EDGE_CURVE('',#5873,#5870,#125,.T.);
#7331=EDGE_CURVE('',#5874,#5875,#3405,.T.);
#7332=EDGE_CURVE('',#5875,#5876,#126,.T.);
#7333=EDGE_CURVE('',#5876,#5877,#3406,.T.);
#7334=EDGE_CURVE('',#5877,#5874,#127,.T.);
#7335=EDGE_CURVE('',#5866,#5876,#3134,.T.);
#7336=EDGE_CURVE('',#5875,#5870,#1011,.T.);
#7337=EDGE_CURVE('',#5873,#5867,#3135,.T.);
#7338=EDGE_CURVE('',#5871,#5874,#1012,.T.);
#7339=EDGE_CURVE('',#5877,#5878,#3136,.T.);
#7340=EDGE_CURVE('',#5878,#5879,#1013,.T.);
#7341=EDGE_CURVE('',#5879,#5872,#3137,.T.);
#7342=EDGE_CURVE('',#5880,#5861,#3407,.T.);
#7343=EDGE_CURVE('',#5879,#5880,#3408,.T.);
#7344=EDGE_CURVE('',#5869,#5878,#3409,.T.);
#7345=EDGE_CURVE('',#5814,#5756,#1014,.T.);
#7346=EDGE_CURVE('',#5757,#5813,#1015,.T.);
#7347=EDGE_CURVE('',#5881,#5881,#1016,.T.);
#7348=EDGE_CURVE('',#5868,#5880,#3410,.T.);
#7349=EDGE_CURVE('',#5829,#5839,#3411,.T.);
#7350=EDGE_CURVE('',#5881,#5882,#3412,.T.);
#7351=EDGE_CURVE('',#5882,#5882,#1017,.T.);
#7352=EDGE_CURVE('',#5883,#5883,#1018,.T.);
#7353=EDGE_CURVE('',#5883,#5755,#3413,.T.);
#7354=EDGE_CURVE('',#5840,#5847,#3414,.T.);
#7355=EDGE_CURVE('',#5843,#5837,#3415,.T.);
#7356=EDGE_CURVE('',#5835,#5845,#3416,.T.);
#7357=EDGE_CURVE('',#5760,#5768,#3417,.T.);
#7358=EDGE_CURVE('',#5763,#5759,#3418,.T.);
#7359=EDGE_CURVE('',#5884,#5885,#3419,.F.);
#7360=EDGE_CURVE('',#5885,#5886,#3420,.T.);
#7361=EDGE_CURVE('',#5886,#5887,#3421,.T.);
#7362=EDGE_CURVE('',#5887,#5884,#3422,.T.);
#7363=EDGE_CURVE('',#5888,#5889,#3423,.T.);
#7364=EDGE_CURVE('',#5889,#5887,#1019,.T.);
#7365=EDGE_CURVE('',#5886,#5888,#1020,.T.);
#7366=EDGE_CURVE('',#5890,#5891,#3424,.F.);
#7367=EDGE_CURVE('',#5891,#5889,#3425,.T.);
#7368=EDGE_CURVE('',#5888,#5890,#3426,.T.);
#7369=EDGE_CURVE('',#5892,#5888,#3427,.T.);
#7370=EDGE_CURVE('',#5893,#5892,#3428,.T.);
#7371=EDGE_CURVE('',#5890,#5893,#3429,.T.);
#7372=EDGE_CURVE('',#5894,#5886,#3430,.T.);
#7373=EDGE_CURVE('',#5892,#5894,#1021,.T.);
#7374=EDGE_CURVE('',#5895,#5885,#3431,.T.);
#7375=EDGE_CURVE('',#5894,#5895,#3432,.T.);
#7376=EDGE_CURVE('',#5895,#5896,#3433,.F.);
#7377=EDGE_CURVE('',#5896,#5897,#3434,.T.);
#7378=EDGE_CURVE('',#5897,#5894,#3435,.T.);
#7379=EDGE_CURVE('',#5898,#5892,#3436,.T.);
#7380=EDGE_CURVE('',#5897,#5898,#1022,.T.);
#7381=EDGE_CURVE('',#5899,#5893,#3437,.F.);
#7382=EDGE_CURVE('',#5898,#5899,#3438,.T.);
#7383=EDGE_CURVE('',#5899,#5896,#3439,.T.);
#7384=EDGE_CURVE('',#5900,#5901,#3440,.T.);
#7385=EDGE_CURVE('',#5902,#5900,#3441,.T.);
#7386=EDGE_CURVE('',#5903,#5902,#3442,.T.);
#7387=EDGE_CURVE('',#5904,#5903,#3443,.T.);
#7388=EDGE_CURVE('',#5905,#5904,#3444,.T.);
#7389=EDGE_CURVE('',#5901,#5905,#3445,.T.);
#7390=EDGE_CURVE('',#5906,#5907,#3446,.F.);
#7391=EDGE_CURVE('',#5907,#5908,#3447,.T.);
#7392=EDGE_CURVE('',#5908,#5909,#3448,.T.);
#7393=EDGE_CURVE('',#5909,#5906,#3449,.T.);
#7394=EDGE_CURVE('',#5910,#5911,#3450,.T.);
#7395=EDGE_CURVE('',#5911,#5909,#1023,.T.);
#7396=EDGE_CURVE('',#5908,#5910,#1024,.T.);
#7397=EDGE_CURVE('',#5912,#5913,#3451,.F.);
#7398=EDGE_CURVE('',#5913,#5911,#3452,.T.);
#7399=EDGE_CURVE('',#5910,#5912,#3453,.T.);
#7400=EDGE_CURVE('',#5914,#5910,#3454,.T.);
#7401=EDGE_CURVE('',#5915,#5914,#3455,.T.);
#7402=EDGE_CURVE('',#5912,#5915,#3456,.T.);
#7403=EDGE_CURVE('',#5916,#5908,#3457,.T.);
#7404=EDGE_CURVE('',#5914,#5916,#1025,.T.);
#7405=EDGE_CURVE('',#5917,#5907,#3458,.T.);
#7406=EDGE_CURVE('',#5916,#5917,#3459,.T.);
#7407=EDGE_CURVE('',#5918,#5919,#3460,.T.);
#7408=EDGE_CURVE('',#5920,#5918,#3461,.T.);
#7409=EDGE_CURVE('',#5919,#5920,#3462,.T.);
#7410=EDGE_CURVE('',#5921,#5922,#3463,.F.);
#7411=EDGE_CURVE('',#5922,#5920,#3464,.T.);
#7412=EDGE_CURVE('',#5918,#5921,#3465,.T.);
#7413=EDGE_CURVE('',#5923,#5924,#3466,.T.);
#7414=EDGE_CURVE('',#5924,#5919,#3467,.T.);
#7415=EDGE_CURVE('',#5920,#5925,#3468,.T.);
#7416=EDGE_CURVE('',#5925,#5923,#3469,.T.);
#7417=EDGE_CURVE('',#5926,#5927,#3470,.T.);
#7418=EDGE_CURVE('',#5927,#5918,#3471,.T.);
#7419=EDGE_CURVE('',#5919,#5928,#3472,.T.);
#7420=EDGE_CURVE('',#5928,#5926,#3473,.T.);
#7421=EDGE_CURVE('',#5929,#5922,#3474,.T.);
#7422=EDGE_CURVE('',#5925,#5929,#3475,.T.);
#7423=EDGE_CURVE('',#5930,#5927,#3476,.T.);
#7424=EDGE_CURVE('',#5921,#5930,#3477,.T.);
#7425=EDGE_CURVE('',#5926,#5931,#3478,.T.);
#7426=EDGE_CURVE('',#5931,#5932,#3479,.T.);
#7427=EDGE_CURVE('',#5932,#5930,#3480,.F.);
#7428=EDGE_CURVE('',#5933,#5933,#1026,.T.);
#7429=EDGE_CURVE('',#5933,#5934,#3481,.T.);
#7430=EDGE_CURVE('',#5934,#5934,#1027,.T.);
#7431=EDGE_CURVE('',#5934,#5935,#3482,.T.);
#7432=EDGE_CURVE('',#5935,#5935,#1028,.T.);
#7433=EDGE_CURVE('',#5884,#5891,#3483,.T.);
#7434=EDGE_CURVE('',#5936,#5936,#1029,.T.);
#7435=EDGE_CURVE('',#5936,#5937,#3484,.T.);
#7436=EDGE_CURVE('',#5937,#5937,#1030,.T.);
#7437=EDGE_CURVE('',#5937,#5938,#3485,.T.);
#7438=EDGE_CURVE('',#5938,#5938,#1031,.T.);
#7439=EDGE_CURVE('',#5906,#5913,#3486,.T.);
#7440=EDGE_CURVE('',#5935,#5939,#3487,.T.);
#7441=EDGE_CURVE('',#5939,#5939,#1032,.T.);
#7442=EDGE_CURVE('',#5940,#5941,#3488,.T.);
#7443=EDGE_CURVE('',#5942,#5940,#3489,.T.);
#7444=EDGE_CURVE('',#5943,#5942,#3490,.T.);
#7445=EDGE_CURVE('',#5944,#5943,#3491,.T.);
#7446=EDGE_CURVE('',#5945,#5944,#3492,.T.);
#7447=EDGE_CURVE('',#5941,#5945,#3493,.T.);
#7448=EDGE_CURVE('',#5903,#5946,#3494,.T.);
#7449=EDGE_CURVE('',#5946,#5947,#3495,.T.);
#7450=EDGE_CURVE('',#5904,#5947,#3496,.T.);
#7451=EDGE_CURVE('',#5902,#5948,#3497,.T.);
#7452=EDGE_CURVE('',#5948,#5946,#3498,.T.);
#7453=EDGE_CURVE('',#5901,#5949,#3499,.T.);
#7454=EDGE_CURVE('',#5949,#5950,#3500,.T.);
#7455=EDGE_CURVE('',#5950,#5900,#3501,.T.);
#7456=EDGE_CURVE('',#5951,#5949,#3502,.T.);
#7457=EDGE_CURVE('',#5905,#5951,#3503,.T.);
#7458=EDGE_CURVE('',#5950,#5948,#3504,.T.);
#7459=EDGE_CURVE('',#5947,#5951,#3505,.T.);
#7460=EDGE_CURVE('',#5948,#5941,#3506,.T.);
#7461=EDGE_CURVE('',#5946,#5945,#3507,.T.);
#7462=EDGE_CURVE('',#5950,#5940,#3508,.T.);
#7463=EDGE_CURVE('',#5949,#5942,#3509,.T.);
#7464=EDGE_CURVE('',#5938,#5952,#3510,.T.);
#7465=EDGE_CURVE('',#5952,#5952,#1033,.T.);
#7466=EDGE_CURVE('',#5953,#5954,#3511,.T.);
#7467=EDGE_CURVE('',#5955,#5953,#3512,.T.);
#7468=EDGE_CURVE('',#5956,#5955,#3513,.T.);
#7469=EDGE_CURVE('',#5957,#5956,#3514,.T.);
#7470=EDGE_CURVE('',#5958,#5957,#3515,.T.);
#7471=EDGE_CURVE('',#5954,#5958,#3516,.T.);
#7472=EDGE_CURVE('',#5959,#5915,#3517,.F.);
#7473=EDGE_CURVE('',#5914,#5960,#3518,.T.);
#7474=EDGE_CURVE('',#5960,#5959,#3519,.T.);
#7475=EDGE_CURVE('',#5916,#5961,#3520,.T.);
#7476=EDGE_CURVE('',#5961,#5960,#1034,.T.);
#7477=EDGE_CURVE('',#5917,#5962,#3521,.F.);
#7478=EDGE_CURVE('',#5962,#5961,#3522,.T.);
#7479=EDGE_CURVE('',#5963,#5964,#3523,.T.);
#7480=EDGE_CURVE('',#5964,#5965,#3524,.T.);
#7481=EDGE_CURVE('',#5965,#5966,#3525,.T.);
#7482=EDGE_CURVE('',#5963,#5966,#3526,.T.);
#7483=EDGE_CURVE('',#5964,#5967,#3527,.T.);
#7484=EDGE_CURVE('',#5967,#5968,#3528,.T.);
#7485=EDGE_CURVE('',#5968,#5965,#3529,.T.);
#7486=EDGE_CURVE('',#5969,#5970,#3530,.T.);
#7487=EDGE_CURVE('',#5970,#5971,#3531,.T.);
#7488=EDGE_CURVE('',#5971,#5972,#3532,.T.);
#7489=EDGE_CURVE('',#5972,#5969,#3533,.T.);
#7490=EDGE_CURVE('',#5973,#5971,#3534,.T.);
#7491=EDGE_CURVE('',#5970,#5974,#3535,.T.);
#7492=EDGE_CURVE('',#5974,#5973,#3536,.T.);
#7493=EDGE_CURVE('',#5967,#5969,#3537,.T.);
#7494=EDGE_CURVE('',#5972,#5968,#3538,.T.);
#7495=EDGE_CURVE('',#5966,#5973,#3539,.T.);
#7496=EDGE_CURVE('',#5974,#5963,#3540,.T.);
#7497=EDGE_CURVE('',#5968,#5954,#3541,.T.);
#7498=EDGE_CURVE('',#5965,#5958,#3542,.T.);
#7499=EDGE_CURVE('',#5972,#5953,#3543,.T.);
#7500=EDGE_CURVE('',#5971,#5955,#3544,.T.);
#7501=EDGE_CURVE('',#5959,#5962,#3545,.T.);
#7502=EDGE_CURVE('',#5975,#5976,#3546,.T.);
#7503=EDGE_CURVE('',#5977,#5975,#3547,.T.);
#7504=EDGE_CURVE('',#5976,#5977,#3548,.T.);
#7505=EDGE_CURVE('',#5978,#5979,#3549,.F.);
#7506=EDGE_CURVE('',#5979,#5977,#3550,.T.);
#7507=EDGE_CURVE('',#5975,#5978,#3551,.T.);
#7508=EDGE_CURVE('',#5980,#5981,#3552,.T.);
#7509=EDGE_CURVE('',#5982,#5980,#3553,.T.);
#7510=EDGE_CURVE('',#5981,#5982,#3554,.T.);
#7511=EDGE_CURVE('',#5983,#5984,#3555,.F.);
#7512=EDGE_CURVE('',#5984,#5982,#3556,.T.);
#7513=EDGE_CURVE('',#5980,#5983,#3557,.T.);
#7514=EDGE_CURVE('',#5985,#5986,#3558,.T.);
#7515=EDGE_CURVE('',#5986,#5981,#3559,.T.);
#7516=EDGE_CURVE('',#5982,#5987,#3560,.T.);
#7517=EDGE_CURVE('',#5987,#5985,#3561,.T.);
#7518=EDGE_CURVE('',#5981,#5976,#3562,.T.);
#7519=EDGE_CURVE('',#5977,#5980,#3563,.T.);
#7520=EDGE_CURVE('',#5988,#5989,#3564,.T.);
#7521=EDGE_CURVE('',#5989,#5975,#3565,.T.);
#7522=EDGE_CURVE('',#5976,#5990,#3566,.T.);
#7523=EDGE_CURVE('',#5990,#5988,#3567,.T.);
#7524=EDGE_CURVE('',#5983,#5979,#3568,.T.);
#7525=EDGE_CURVE('',#5991,#5989,#3569,.T.);
#7526=EDGE_CURVE('',#5978,#5991,#3570,.T.);
#7527=EDGE_CURVE('',#5988,#5992,#3571,.T.);
#7528=EDGE_CURVE('',#5992,#5993,#3572,.T.);
#7529=EDGE_CURVE('',#5991,#5993,#3573,.T.);
#7530=EDGE_CURVE('',#5994,#5995,#3574,.T.);
#7531=EDGE_CURVE('',#5996,#5994,#3575,.T.);
#7532=EDGE_CURVE('',#5995,#5996,#3576,.T.);
#7533=EDGE_CURVE('',#5997,#5998,#3577,.F.);
#7534=EDGE_CURVE('',#5998,#5996,#3578,.T.);
#7535=EDGE_CURVE('',#5994,#5997,#3579,.T.);
#7536=EDGE_CURVE('',#5999,#6000,#3580,.T.);
#7537=EDGE_CURVE('',#6001,#5999,#3581,.T.);
#7538=EDGE_CURVE('',#6000,#6001,#3582,.T.);
#7539=EDGE_CURVE('',#6002,#6003,#3583,.F.);
#7540=EDGE_CURVE('',#6003,#6001,#3584,.T.);
#7541=EDGE_CURVE('',#5999,#6002,#3585,.T.);
#7542=EDGE_CURVE('',#6004,#6005,#3586,.T.);
#7543=EDGE_CURVE('',#6005,#6000,#3587,.T.);
#7544=EDGE_CURVE('',#6001,#6006,#3588,.T.);
#7545=EDGE_CURVE('',#6006,#6004,#3589,.T.);
#7546=EDGE_CURVE('',#6000,#5995,#3590,.T.);
#7547=EDGE_CURVE('',#5996,#5999,#3591,.T.);
#7548=EDGE_CURVE('',#6007,#6008,#3592,.T.);
#7549=EDGE_CURVE('',#6008,#5994,#3593,.T.);
#7550=EDGE_CURVE('',#5995,#6009,#3594,.T.);
#7551=EDGE_CURVE('',#6009,#6007,#3595,.T.);
#7552=EDGE_CURVE('',#6002,#5998,#3596,.T.);
#7553=EDGE_CURVE('',#6010,#6008,#3597,.T.);
#7554=EDGE_CURVE('',#5997,#6010,#3598,.T.);
#7555=EDGE_CURVE('',#6007,#6011,#3599,.T.);
#7556=EDGE_CURVE('',#6011,#6012,#3600,.T.);
#7557=EDGE_CURVE('',#6010,#6012,#3601,.T.);
#7558=EDGE_CURVE('',#5928,#6013,#3602,.T.);
#7559=EDGE_CURVE('',#6013,#6014,#3603,.T.);
#7560=EDGE_CURVE('',#6014,#6015,#3604,.T.);
#7561=EDGE_CURVE('',#6015,#5931,#3605,.T.);
#7562=EDGE_CURVE('',#6016,#6015,#3606,.T.);
#7563=EDGE_CURVE('',#5932,#6016,#3607,.T.);
#7564=EDGE_CURVE('',#6014,#6017,#3608,.T.);
#7565=EDGE_CURVE('',#6017,#6018,#3609,.T.);
#7566=EDGE_CURVE('',#6016,#6018,#3610,.T.);
#7567=EDGE_CURVE('',#6019,#6020,#3611,.T.);
#7568=EDGE_CURVE('',#6020,#6021,#3612,.F.);
#7569=EDGE_CURVE('',#6021,#6022,#3613,.T.);
#7570=EDGE_CURVE('',#6022,#6019,#3614,.T.);
#7571=EDGE_CURVE('',#6022,#6023,#3615,.T.);
#7572=EDGE_CURVE('',#6023,#6024,#3616,.F.);
#7573=EDGE_CURVE('',#6024,#6019,#3617,.T.);
#7574=EDGE_CURVE('',#6019,#6025,#3618,.T.);
#7575=EDGE_CURVE('',#6025,#6026,#3619,.T.);
#7576=EDGE_CURVE('',#6020,#6026,#3620,.T.);
#7577=EDGE_CURVE('',#6024,#6027,#3621,.T.);
#7578=EDGE_CURVE('',#6027,#6025,#3622,.T.);
#7579=EDGE_CURVE('',#6028,#6021,#3623,.T.);
#7580=EDGE_CURVE('',#6020,#6029,#3624,.T.);
#7581=EDGE_CURVE('',#6029,#6028,#3625,.T.);
#7582=EDGE_CURVE('',#6029,#6024,#3626,.T.);
#7583=EDGE_CURVE('',#6023,#6028,#3627,.T.);
#7584=EDGE_CURVE('',#6030,#6031,#3628,.T.);
#7585=EDGE_CURVE('',#6032,#6030,#3629,.T.);
#7586=EDGE_CURVE('',#6033,#6032,#1035,.T.);
#7587=EDGE_CURVE('',#6034,#6033,#3630,.T.);
#7588=EDGE_CURVE('',#5993,#6034,#3631,.T.);
#7589=EDGE_CURVE('',#6035,#5992,#3632,.T.);
#7590=EDGE_CURVE('',#6036,#6035,#3633,.T.);
#7591=EDGE_CURVE('',#6012,#6036,#3634,.T.);
#7592=EDGE_CURVE('',#6037,#6011,#3635,.T.);
#7593=EDGE_CURVE('',#6038,#6037,#3636,.T.);
#7594=EDGE_CURVE('',#6018,#6038,#3637,.T.);
#7595=EDGE_CURVE('',#6039,#6017,#3638,.T.);
#7596=EDGE_CURVE('',#6040,#6039,#3639,.T.);
#7597=EDGE_CURVE('',#6041,#6040,#3640,.T.);
#7598=EDGE_CURVE('',#6042,#6041,#3641,.T.);
#7599=EDGE_CURVE('',#6043,#6042,#1036,.T.);
#7600=EDGE_CURVE('',#6031,#6043,#3642,.T.);
#7601=EDGE_CURVE('',#6044,#6030,#3643,.T.);
#7602=EDGE_CURVE('',#6031,#6045,#3644,.T.);
#7603=EDGE_CURVE('',#6045,#6044,#3645,.T.);
#7604=EDGE_CURVE('',#6046,#6047,#3646,.T.);
#7605=EDGE_CURVE('',#6047,#6030,#1037,.T.);
#7606=EDGE_CURVE('',#6044,#6046,#1038,.T.);
#7607=EDGE_CURVE('',#6048,#6049,#3647,.T.);
#7608=EDGE_CURVE('',#6049,#6047,#3648,.T.);
#7609=EDGE_CURVE('',#6046,#6048,#3649,.T.);
#7610=EDGE_CURVE('',#6050,#6051,#3650,.T.);
#7611=EDGE_CURVE('',#6051,#6049,#1039,.T.);
#7612=EDGE_CURVE('',#6048,#6050,#1040,.T.);
#7613=EDGE_CURVE('',#6052,#6053,#3651,.T.);
#7614=EDGE_CURVE('',#6053,#6051,#3652,.T.);
#7615=EDGE_CURVE('',#6050,#6052,#3653,.T.);
#7616=EDGE_CURVE('',#6054,#6055,#3654,.T.);
#7617=EDGE_CURVE('',#6055,#6053,#1041,.T.);
#7618=EDGE_CURVE('',#6052,#6054,#1042,.T.);
#7619=EDGE_CURVE('',#6056,#6057,#3655,.T.);
#7620=EDGE_CURVE('',#6057,#6055,#3656,.T.);
#7621=EDGE_CURVE('',#6054,#6056,#3657,.T.);
#7622=EDGE_CURVE('',#6031,#6057,#1043,.T.);
#7623=EDGE_CURVE('',#6056,#6045,#1044,.T.);
#7624=EDGE_CURVE('',#6055,#6058,#3658,.T.);
#7625=EDGE_CURVE('',#6059,#6058,#1045,.T.);
#7626=EDGE_CURVE('',#6059,#6053,#3659,.T.);
#7627=EDGE_CURVE('',#6060,#6057,#3660,.T.);
#7628=EDGE_CURVE('',#6058,#6060,#3661,.T.);
#7629=EDGE_CURVE('',#6061,#6061,#1046,.T.);
#7630=EDGE_CURVE('',#6062,#6043,#128,.T.);
#7631=EDGE_CURVE('',#6063,#6062,#129,.T.);
#7632=EDGE_CURVE('',#6042,#6063,#130,.T.);
#7633=EDGE_CURVE('',#6060,#6041,#1047,.T.);
#7634=EDGE_CURVE('',#6064,#6016,#3662,.T.);
#7635=EDGE_CURVE('',#6038,#6064,#3663,.T.);
#7636=EDGE_CURVE('',#6036,#6065,#3664,.T.);
#7637=EDGE_CURVE('',#6065,#6010,#3665,.T.);
#7638=EDGE_CURVE('',#5987,#6065,#3666,.T.);
#7639=EDGE_CURVE('',#6035,#5985,#3667,.T.);
#7640=EDGE_CURVE('',#6034,#6066,#3668,.T.);
#7641=EDGE_CURVE('',#6066,#5991,#3669,.T.);
#7642=EDGE_CURVE('',#6034,#6067,#1048,.T.);
#7643=EDGE_CURVE('',#6067,#6068,#3670,.T.);
#7644=EDGE_CURVE('',#6068,#6066,#1049,.T.);
#7645=EDGE_CURVE('',#6069,#6070,#3671,.T.);
#7646=EDGE_CURVE('',#6070,#6068,#3672,.T.);
#7647=EDGE_CURVE('',#6067,#6069,#3673,.T.);
#7648=EDGE_CURVE('',#6069,#6071,#1050,.T.);
#7649=EDGE_CURVE('',#6071,#6072,#3674,.T.);
#7650=EDGE_CURVE('',#6072,#6070,#1051,.T.);
#7651=EDGE_CURVE('',#6059,#6073,#3675,.T.);
#7652=EDGE_CURVE('',#6073,#6072,#3676,.T.);
#7653=EDGE_CURVE('',#6071,#6059,#3677,.T.);
#7654=EDGE_CURVE('',#6058,#6074,#3678,.T.);
#7655=EDGE_CURVE('',#6074,#6073,#1052,.T.);
#7656=EDGE_CURVE('',#6060,#6075,#3679,.T.);
#7657=EDGE_CURVE('',#6075,#6074,#3680,.T.);
#7658=EDGE_CURVE('',#6041,#6076,#3681,.T.);
#7659=EDGE_CURVE('',#6076,#6075,#1053,.T.);
#7660=EDGE_CURVE('',#5929,#6076,#3682,.T.);
#7661=EDGE_CURVE('',#6040,#5929,#3683,.T.);
#7662=EDGE_CURVE('',#6039,#5923,#3684,.T.);
#7663=EDGE_CURVE('',#5990,#5986,#3685,.T.);
#7664=EDGE_CURVE('',#6013,#5924,#3686,.T.);
#7665=EDGE_CURVE('',#6006,#6064,#3687,.T.);
#7666=EDGE_CURVE('',#6037,#6004,#3688,.T.);
#7667=EDGE_CURVE('',#6009,#6005,#3689,.T.);
#7668=EDGE_CURVE('',#6051,#6071,#3690,.T.);
#7669=EDGE_CURVE('',#6069,#6049,#3691,.T.);
#7670=EDGE_CURVE('',#6047,#6067,#3692,.T.);
#7671=EDGE_CURVE('',#6077,#6033,#131,.T.);
#7672=EDGE_CURVE('',#6078,#6077,#132,.T.);
#7673=EDGE_CURVE('',#6032,#6078,#133,.T.);
#7674=EDGE_CURVE('',#6064,#6003,#3693,.T.);
#7675=EDGE_CURVE('',#6065,#5984,#3694,.T.);
#7676=EDGE_CURVE('',#6079,#6063,#3695,.T.);
#7677=EDGE_CURVE('',#6062,#6080,#3696,.T.);
#7678=EDGE_CURVE('',#6080,#6079,#134,.T.);
#7679=EDGE_CURVE('',#6042,#6081,#3697,.T.);
#7680=EDGE_CURVE('',#6081,#6082,#1054,.T.);
#7681=EDGE_CURVE('',#6082,#6083,#1055,.T.);
#7682=EDGE_CURVE('',#6083,#6043,#3698,.T.);
#7683=EDGE_CURVE('',#6079,#6081,#135,.T.);
#7684=EDGE_CURVE('',#6083,#6080,#136,.T.);
#7685=EDGE_CURVE('',#6082,#6084,#3699,.T.);
#7686=EDGE_CURVE('',#6084,#6084,#1056,.T.);
#7687=EDGE_CURVE('',#6085,#6078,#3700,.T.);
#7688=EDGE_CURVE('',#6077,#6086,#3701,.T.);
#7689=EDGE_CURVE('',#6086,#6087,#137,.T.);
#7690=EDGE_CURVE('',#6087,#6085,#138,.T.);
#7691=EDGE_CURVE('',#6032,#6088,#3702,.T.);
#7692=EDGE_CURVE('',#6088,#6089,#1057,.T.);
#7693=EDGE_CURVE('',#6089,#6033,#3703,.T.);
#7694=EDGE_CURVE('',#6085,#6088,#139,.T.);
#7695=EDGE_CURVE('',#6089,#6086,#140,.T.);
#7696=EDGE_CURVE('',#6087,#6090,#3704,.T.);
#7697=EDGE_CURVE('',#6090,#6090,#1058,.T.);
#7698=EDGE_CURVE('',#6061,#6091,#3705,.T.);
#7699=EDGE_CURVE('',#6091,#6091,#1059,.T.);
#7700=EDGE_CURVE('',#6091,#6092,#3706,.T.);
#7701=EDGE_CURVE('',#6092,#6092,#1060,.T.);
#7702=EDGE_CURVE('',#6093,#6093,#1061,.T.);
#7703=EDGE_CURVE('',#6093,#6092,#3707,.T.);
#7704=EDGE_CURVE('',#6026,#6094,#3708,.T.);
#7705=EDGE_CURVE('',#6029,#6094,#3709,.T.);
#7706=EDGE_CURVE('',#5973,#5956,#3710,.T.);
#7707=EDGE_CURVE('',#5966,#5957,#3711,.T.);
#7708=EDGE_CURVE('',#5951,#5943,#3712,.T.);
#7709=EDGE_CURVE('',#5947,#5944,#3713,.T.);
#7710=EDGE_CURVE('',#6094,#6027,#3714,.T.);
#7711=EDGE_CURVE('',#6095,#6095,#1062,.T.);
#7712=EDGE_CURVE('',#6095,#6096,#3715,.T.);
#7713=EDGE_CURVE('',#6096,#6096,#1063,.T.);
#7714=EDGE_CURVE('',#6097,#6097,#1064,.T.);
#7715=EDGE_CURVE('',#6097,#6096,#3716,.T.);
#7716=EDGE_CURVE('',#6098,#6099,#3717,.T.);
#7717=EDGE_CURVE('',#6100,#6098,#1065,.T.);
#7718=EDGE_CURVE('',#6101,#6100,#3718,.T.);
#7719=EDGE_CURVE('',#6102,#6101,#1066,.T.);
#7720=EDGE_CURVE('',#6103,#6102,#3719,.T.);
#7721=EDGE_CURVE('',#6104,#6103,#1067,.T.);
#7722=EDGE_CURVE('',#6105,#6104,#3720,.T.);
#7723=EDGE_CURVE('',#6099,#6105,#1068,.T.);
#7724=EDGE_CURVE('',#6106,#6106,#1069,.T.);
#7725=EDGE_CURVE('',#6107,#6107,#1070,.T.);
#7726=EDGE_CURVE('',#6108,#6108,#1071,.T.);
#7727=EDGE_CURVE('',#6108,#6097,#3721,.T.);
#7728=EDGE_CURVE('',#6109,#6110,#3722,.T.);
#7729=EDGE_CURVE('',#6111,#6109,#1072,.T.);
#7730=EDGE_CURVE('',#6112,#6111,#3723,.T.);
#7731=EDGE_CURVE('',#6113,#6112,#1073,.T.);
#7732=EDGE_CURVE('',#6114,#6113,#3724,.T.);
#7733=EDGE_CURVE('',#6115,#6114,#1074,.T.);
#7734=EDGE_CURVE('',#6116,#6115,#3725,.T.);
#7735=EDGE_CURVE('',#6110,#6116,#1075,.T.);
#7736=EDGE_CURVE('',#6117,#6117,#1076,.T.);
#7737=EDGE_CURVE('',#6118,#6118,#1077,.T.);
#7738=EDGE_CURVE('',#6119,#6098,#3726,.T.);
#7739=EDGE_CURVE('',#6099,#6120,#3727,.T.);
#7740=EDGE_CURVE('',#6120,#6119,#3728,.T.);
#7741=EDGE_CURVE('',#6119,#6121,#1078,.T.);
#7742=EDGE_CURVE('',#6121,#6100,#3729,.T.);
#7743=EDGE_CURVE('',#6122,#6101,#3730,.T.);
#7744=EDGE_CURVE('',#6121,#6122,#3731,.T.);
#7745=EDGE_CURVE('',#6122,#6123,#1079,.T.);
#7746=EDGE_CURVE('',#6123,#6102,#3732,.T.);
#7747=EDGE_CURVE('',#6124,#6103,#3733,.T.);
#7748=EDGE_CURVE('',#6123,#6124,#3734,.T.);
#7749=EDGE_CURVE('',#6124,#6125,#1080,.T.);
#7750=EDGE_CURVE('',#6125,#6104,#3735,.T.);
#7751=EDGE_CURVE('',#6126,#6105,#3736,.T.);
#7752=EDGE_CURVE('',#6125,#6126,#3737,.T.);
#7753=EDGE_CURVE('',#6126,#6120,#1081,.T.);
#7754=EDGE_CURVE('',#6122,#6127,#3738,.T.);
#7755=EDGE_CURVE('',#6128,#6127,#1082,.T.);
#7756=EDGE_CURVE('',#6128,#6123,#3739,.T.);
#7757=EDGE_CURVE('',#6129,#6121,#3740,.T.);
#7758=EDGE_CURVE('',#6127,#6129,#3741,.T.);
#7759=EDGE_CURVE('',#6119,#6130,#3742,.T.);
#7760=EDGE_CURVE('',#6129,#6130,#1083,.T.);
#7761=EDGE_CURVE('',#6131,#6120,#3743,.T.);
#7762=EDGE_CURVE('',#6130,#6131,#3744,.T.);
#7763=EDGE_CURVE('',#6128,#6132,#3745,.T.);
#7764=EDGE_CURVE('',#6132,#6133,#3746,.T.);
#7765=EDGE_CURVE('',#6133,#6134,#3747,.T.);
#7766=EDGE_CURVE('',#6134,#6128,#3748,.T.);
#7767=EDGE_CURVE('',#6127,#6135,#3749,.T.);
#7768=EDGE_CURVE('',#6135,#6132,#1084,.T.);
#7769=EDGE_CURVE('',#6129,#6136,#3750,.T.);
#7770=EDGE_CURVE('',#6136,#6135,#3751,.T.);
#7771=EDGE_CURVE('',#6130,#6137,#3752,.T.);
#7772=EDGE_CURVE('',#6137,#6136,#1085,.T.);
#7773=EDGE_CURVE('',#6131,#6138,#3753,.T.);
#7774=EDGE_CURVE('',#6138,#6137,#3754,.T.);
#7775=EDGE_CURVE('',#6139,#6140,#3755,.T.);
#7776=EDGE_CURVE('',#6140,#6138,#1086,.T.);
#7777=EDGE_CURVE('',#6131,#6139,#1087,.T.);
#7778=EDGE_CURVE('',#6141,#6142,#3756,.T.);
#7779=EDGE_CURVE('',#6142,#6140,#3757,.T.);
#7780=EDGE_CURVE('',#6139,#6141,#3758,.T.);
#7781=EDGE_CURVE('',#6133,#6142,#1088,.T.);
#7782=EDGE_CURVE('',#6141,#6134,#1089,.T.);
#7783=EDGE_CURVE('',#6143,#6140,#3759,.T.);
#7784=EDGE_CURVE('',#6144,#6143,#1090,.T.);
#7785=EDGE_CURVE('',#6144,#6138,#3760,.T.);
#7786=EDGE_CURVE('',#6145,#6142,#3761,.T.);
#7787=EDGE_CURVE('',#6143,#6145,#3762,.T.);
#7788=EDGE_CURVE('',#6146,#6133,#3763,.T.);
#7789=EDGE_CURVE('',#6145,#6146,#1091,.T.);
#7790=EDGE_CURVE('',#6147,#6132,#3764,.T.);
#7791=EDGE_CURVE('',#6146,#6147,#3765,.T.);
#7792=EDGE_CURVE('',#6124,#6134,#3766,.T.);
#7793=EDGE_CURVE('',#6110,#6146,#3767,.T.);
#7794=EDGE_CURVE('',#6147,#6109,#3768,.T.);
#7795=EDGE_CURVE('',#6116,#6145,#3769,.T.);
#7796=EDGE_CURVE('',#6115,#6143,#3770,.T.);
#7797=EDGE_CURVE('',#6114,#6144,#3771,.T.);
#7798=EDGE_CURVE('',#6113,#6148,#3772,.T.);
#7799=EDGE_CURVE('',#6148,#6144,#3773,.T.);
#7800=EDGE_CURVE('',#6112,#6149,#3774,.T.);
#7801=EDGE_CURVE('',#6149,#6148,#1092,.T.);
#7802=EDGE_CURVE('',#6111,#6150,#3775,.T.);
#7803=EDGE_CURVE('',#6150,#6149,#3776,.T.);
#7804=EDGE_CURVE('',#6147,#6150,#1093,.T.);
#7805=EDGE_CURVE('',#6148,#6137,#3777,.T.);
#7806=EDGE_CURVE('',#6149,#6136,#3778,.T.);
#7807=EDGE_CURVE('',#6135,#6150,#3779,.T.);
#7808=EDGE_CURVE('',#6118,#6106,#3780,.T.);
#7809=EDGE_CURVE('',#6117,#6107,#3781,.T.);
#7810=EDGE_CURVE('',#6126,#6139,#3782,.T.);
#7811=EDGE_CURVE('',#6141,#6125,#3783,.T.);
#7812=EDGE_CURVE('',#6151,#6152,#3784,.T.);
#7813=EDGE_CURVE('',#6151,#6153,#3785,.T.);
#7814=EDGE_CURVE('',#6154,#6153,#3786,.T.);
#7815=EDGE_CURVE('',#6152,#6154,#3787,.T.);
#7816=EDGE_CURVE('',#6152,#6155,#3788,.T.);
#7817=EDGE_CURVE('',#6156,#6154,#3789,.T.);
#7818=EDGE_CURVE('',#6155,#6156,#3790,.T.);
#7819=EDGE_CURVE('',#6155,#6157,#3791,.T.);
#7820=EDGE_CURVE('',#6158,#6156,#3792,.T.);
#7821=EDGE_CURVE('',#6157,#6158,#3793,.T.);
#7822=EDGE_CURVE('',#6157,#6151,#3794,.T.);
#7823=EDGE_CURVE('',#6153,#6158,#3795,.T.);
#7824=EDGE_CURVE('',#6159,#6160,#3796,.T.);
#7825=EDGE_CURVE('',#6159,#6161,#3797,.T.);
#7826=EDGE_CURVE('',#6162,#6161,#3798,.T.);
#7827=EDGE_CURVE('',#6160,#6162,#3799,.T.);
#7828=EDGE_CURVE('',#6160,#6163,#3800,.T.);
#7829=EDGE_CURVE('',#6164,#6162,#3801,.T.);
#7830=EDGE_CURVE('',#6163,#6164,#3802,.T.);
#7831=EDGE_CURVE('',#6163,#6165,#3803,.T.);
#7832=EDGE_CURVE('',#6166,#6164,#3804,.T.);
#7833=EDGE_CURVE('',#6165,#6166,#3805,.T.);
#7834=EDGE_CURVE('',#6165,#6159,#3806,.T.);
#7835=EDGE_CURVE('',#6161,#6166,#3807,.T.);
#7836=EDGE_CURVE('',#6167,#6168,#3808,.T.);
#7837=EDGE_CURVE('',#6167,#6169,#3809,.T.);
#7838=EDGE_CURVE('',#6170,#6169,#3810,.T.);
#7839=EDGE_CURVE('',#6168,#6170,#3811,.T.);
#7840=EDGE_CURVE('',#6168,#6171,#3812,.T.);
#7841=EDGE_CURVE('',#6172,#6170,#3813,.T.);
#7842=EDGE_CURVE('',#6171,#6172,#3814,.T.);
#7843=EDGE_CURVE('',#6171,#6173,#3815,.T.);
#7844=EDGE_CURVE('',#6174,#6172,#3816,.T.);
#7845=EDGE_CURVE('',#6173,#6174,#3817,.T.);
#7846=EDGE_CURVE('',#6173,#6167,#3818,.T.);
#7847=EDGE_CURVE('',#6169,#6174,#3819,.T.);
#7848=EDGE_CURVE('',#6175,#6176,#3820,.T.);
#7849=EDGE_CURVE('',#6175,#6177,#3821,.T.);
#7850=EDGE_CURVE('',#6178,#6177,#3822,.T.);
#7851=EDGE_CURVE('',#6176,#6178,#3823,.T.);
#7852=EDGE_CURVE('',#6176,#6179,#3824,.T.);
#7853=EDGE_CURVE('',#6180,#6178,#3825,.T.);
#7854=EDGE_CURVE('',#6179,#6180,#3826,.T.);
#7855=EDGE_CURVE('',#6179,#6181,#3827,.T.);
#7856=EDGE_CURVE('',#6182,#6180,#3828,.T.);
#7857=EDGE_CURVE('',#6181,#6182,#3829,.T.);
#7858=EDGE_CURVE('',#6181,#6175,#3830,.T.);
#7859=EDGE_CURVE('',#6177,#6182,#3831,.T.);
#7860=EDGE_CURVE('',#6183,#6184,#3832,.T.);
#7861=EDGE_CURVE('',#6185,#6183,#3833,.T.);
#7862=EDGE_CURVE('',#6184,#6185,#3834,.T.);
#7863=EDGE_CURVE('',#6186,#6187,#3835,.T.);
#7864=EDGE_CURVE('',#6188,#6186,#3836,.T.);
#7865=EDGE_CURVE('',#6187,#6188,#3837,.T.);
#7866=EDGE_CURVE('',#6189,#6190,#3838,.T.);
#7867=EDGE_CURVE('',#6191,#6189,#3839,.T.);
#7868=EDGE_CURVE('',#6190,#6191,#3840,.T.);
#7869=EDGE_CURVE('',#6192,#6193,#3841,.T.);
#7870=EDGE_CURVE('',#6194,#6192,#3842,.T.);
#7871=EDGE_CURVE('',#6193,#6194,#3843,.T.);
#7872=EDGE_CURVE('',#6195,#6196,#3844,.T.);
#7873=EDGE_CURVE('',#6197,#6195,#3845,.T.);
#7874=EDGE_CURVE('',#6196,#6197,#3846,.T.);
#7875=EDGE_CURVE('',#6198,#6199,#3847,.T.);
#7876=EDGE_CURVE('',#6200,#6198,#3848,.T.);
#7877=EDGE_CURVE('',#6199,#6200,#3849,.T.);
#7878=EDGE_CURVE('',#6201,#6202,#3850,.T.);
#7879=EDGE_CURVE('',#6203,#6201,#3851,.T.);
#7880=EDGE_CURVE('',#6202,#6203,#3852,.T.);
#7881=EDGE_CURVE('',#6191,#6203,#3853,.T.);
#7882=EDGE_CURVE('',#6201,#6190,#3854,.T.);
#7883=EDGE_CURVE('',#6204,#6205,#3855,.T.);
#7884=EDGE_CURVE('',#6206,#6204,#3856,.T.);
#7885=EDGE_CURVE('',#6205,#6206,#3857,.T.);
#7886=EDGE_CURVE('',#6204,#6197,#3858,.T.);
#7887=EDGE_CURVE('',#6195,#6206,#3859,.T.);
#7888=EDGE_CURVE('',#6198,#6205,#3860,.T.);
#7889=EDGE_CURVE('',#6206,#6200,#3861,.T.);
#7890=EDGE_CURVE('',#6203,#6204,#3862,.T.);
#7891=EDGE_CURVE('',#6205,#6202,#3863,.T.);
#7892=EDGE_CURVE('',#6192,#6201,#3864,.T.);
#7893=EDGE_CURVE('',#6202,#6194,#3865,.T.);
#7894=EDGE_CURVE('',#6187,#6199,#3866,.T.);
#7895=EDGE_CURVE('',#6200,#6186,#3867,.T.);
#7896=EDGE_CURVE('',#6199,#6193,#3868,.T.);
#7897=EDGE_CURVE('',#6194,#6198,#3869,.T.);
#7898=EDGE_CURVE('',#6197,#6191,#3870,.T.);
#7899=EDGE_CURVE('',#6189,#6196,#3871,.T.);
#7900=EDGE_CURVE('',#6186,#6195,#3872,.T.);
#7901=EDGE_CURVE('',#6196,#6188,#3873,.T.);
#7902=EDGE_CURVE('',#6193,#6184,#3874,.T.);
#7903=EDGE_CURVE('',#6185,#6192,#3875,.T.);
#7904=EDGE_CURVE('',#6183,#6189,#3876,.T.);
#7905=EDGE_CURVE('',#6190,#6185,#3877,.T.);
#7906=EDGE_CURVE('',#6184,#6187,#3878,.T.);
#7907=EDGE_CURVE('',#6188,#6183,#3879,.T.);
#7908=EDGE_CURVE('',#6207,#6207,#1094,.T.);
#7909=EDGE_CURVE('',#6208,#6208,#1095,.T.);
#7910=EDGE_CURVE('',#6208,#6207,#3880,.T.);
#7911=EDGE_CURVE('',#6209,#6210,#3881,.T.);
#7912=EDGE_CURVE('',#6209,#6211,#141,.T.);
#7913=EDGE_CURVE('',#6211,#6212,#1096,.T.);
#7914=EDGE_CURVE('',#6212,#6210,#142,.T.);
#7915=EDGE_CURVE('',#6213,#6214,#3882,.T.);
#7916=EDGE_CURVE('',#6213,#6209,#143,.T.);
#7917=EDGE_CURVE('',#6210,#6214,#144,.T.);
#7918=EDGE_CURVE('',#6215,#6216,#3883,.T.);
#7919=EDGE_CURVE('',#6215,#6213,#145,.T.);
#7920=EDGE_CURVE('',#6214,#6216,#146,.T.);
#7921=EDGE_CURVE('',#6217,#6218,#3884,.T.);
#7922=EDGE_CURVE('',#6217,#6215,#147,.T.);
#7923=EDGE_CURVE('',#6216,#6218,#148,.T.);
#7924=EDGE_CURVE('',#6219,#6220,#3885,.T.);
#7925=EDGE_CURVE('',#6219,#6217,#149,.T.);
#7926=EDGE_CURVE('',#6218,#6220,#150,.T.);
#7927=EDGE_CURVE('',#6221,#6222,#3886,.T.);
#7928=EDGE_CURVE('',#6221,#6219,#151,.T.);
#7929=EDGE_CURVE('',#6220,#6222,#152,.T.);
#7930=EDGE_CURVE('',#6223,#6224,#3887,.T.);
#7931=EDGE_CURVE('',#6223,#6221,#153,.T.);
#7932=EDGE_CURVE('',#6222,#6224,#154,.T.);
#7933=EDGE_CURVE('',#6225,#6226,#3888,.T.);
#7934=EDGE_CURVE('',#6225,#6223,#155,.T.);
#7935=EDGE_CURVE('',#6224,#6226,#156,.T.);
#7936=EDGE_CURVE('',#6227,#6228,#3889,.T.);
#7937=EDGE_CURVE('',#6227,#6225,#157,.T.);
#7938=EDGE_CURVE('',#6226,#6228,#158,.T.);
#7939=EDGE_CURVE('',#6229,#6230,#3890,.T.);
#7940=EDGE_CURVE('',#6229,#6227,#159,.T.);
#7941=EDGE_CURVE('',#6228,#6230,#160,.T.);
#7942=EDGE_CURVE('',#6231,#6232,#3891,.T.);
#7943=EDGE_CURVE('',#6231,#6229,#161,.T.);
#7944=EDGE_CURVE('',#6230,#6232,#162,.T.);
#7945=EDGE_CURVE('',#6233,#6234,#3892,.T.);
#7946=EDGE_CURVE('',#6233,#6231,#163,.T.);
#7947=EDGE_CURVE('',#6232,#6234,#164,.T.);
#7948=EDGE_CURVE('',#6235,#6236,#3893,.T.);
#7949=EDGE_CURVE('',#6235,#6233,#165,.T.);
#7950=EDGE_CURVE('',#6234,#6236,#166,.T.);
#7951=EDGE_CURVE('',#6237,#6238,#3894,.T.);
#7952=EDGE_CURVE('',#6237,#6235,#167,.T.);
#7953=EDGE_CURVE('',#6236,#6238,#168,.T.);
#7954=EDGE_CURVE('',#6239,#6240,#3895,.T.);
#7955=EDGE_CURVE('',#6239,#6237,#169,.T.);
#7956=EDGE_CURVE('',#6238,#6240,#170,.T.);
#7957=EDGE_CURVE('',#6241,#6242,#3896,.T.);
#7958=EDGE_CURVE('',#6241,#6239,#171,.T.);
#7959=EDGE_CURVE('',#6240,#6242,#172,.T.);
#7960=EDGE_CURVE('',#6243,#6244,#3897,.T.);
#7961=EDGE_CURVE('',#6243,#6241,#173,.T.);
#7962=EDGE_CURVE('',#6242,#6244,#174,.T.);
#7963=EDGE_CURVE('',#6245,#6246,#3898,.T.);
#7964=EDGE_CURVE('',#6245,#6243,#175,.T.);
#7965=EDGE_CURVE('',#6244,#6246,#176,.T.);
#7966=EDGE_CURVE('',#6247,#6248,#3899,.T.);
#7967=EDGE_CURVE('',#6247,#6245,#177,.T.);
#7968=EDGE_CURVE('',#6246,#6248,#178,.T.);
#7969=EDGE_CURVE('',#6249,#6250,#3900,.T.);
#7970=EDGE_CURVE('',#6249,#6247,#179,.T.);
#7971=EDGE_CURVE('',#6248,#6250,#180,.T.);
#7972=EDGE_CURVE('',#6251,#6252,#3901,.T.);
#7973=EDGE_CURVE('',#6251,#6249,#181,.T.);
#7974=EDGE_CURVE('',#6250,#6252,#182,.T.);
#7975=EDGE_CURVE('',#6253,#6254,#3902,.T.);
#7976=EDGE_CURVE('',#6253,#6251,#183,.T.);
#7977=EDGE_CURVE('',#6252,#6254,#184,.T.);
#7978=EDGE_CURVE('',#6255,#6256,#3903,.T.);
#7979=EDGE_CURVE('',#6255,#6253,#185,.T.);
#7980=EDGE_CURVE('',#6254,#6256,#186,.T.);
#7981=EDGE_CURVE('',#6257,#6258,#3904,.T.);
#7982=EDGE_CURVE('',#6257,#6255,#187,.T.);
#7983=EDGE_CURVE('',#6256,#6258,#188,.T.);
#7984=EDGE_CURVE('',#6259,#6260,#3905,.T.);
#7985=EDGE_CURVE('',#6259,#6257,#189,.T.);
#7986=EDGE_CURVE('',#6258,#6260,#190,.T.);
#7987=EDGE_CURVE('',#6261,#6262,#3906,.T.);
#7988=EDGE_CURVE('',#6261,#6259,#191,.T.);
#7989=EDGE_CURVE('',#6260,#6262,#192,.T.);
#7990=EDGE_CURVE('',#6263,#6264,#3907,.T.);
#7991=EDGE_CURVE('',#6263,#6261,#193,.T.);
#7992=EDGE_CURVE('',#6262,#6264,#194,.T.);
#7993=EDGE_CURVE('',#6265,#6266,#3908,.T.);
#7994=EDGE_CURVE('',#6265,#6263,#195,.T.);
#7995=EDGE_CURVE('',#6264,#6266,#196,.T.);
#7996=EDGE_CURVE('',#6267,#6268,#3909,.T.);
#7997=EDGE_CURVE('',#6267,#6269,#197,.T.);
#7998=EDGE_CURVE('',#6270,#6269,#1097,.T.);
#7999=EDGE_CURVE('',#6268,#6270,#198,.T.);
#8000=EDGE_CURVE('',#6271,#6272,#3910,.T.);
#8001=EDGE_CURVE('',#6271,#6267,#199,.T.);
#8002=EDGE_CURVE('',#6272,#6268,#200,.T.);
#8003=EDGE_CURVE('',#6273,#6274,#3911,.T.);
#8004=EDGE_CURVE('',#6273,#6271,#201,.T.);
#8005=EDGE_CURVE('',#6274,#6272,#202,.T.);
#8006=EDGE_CURVE('',#6275,#6276,#3912,.T.);
#8007=EDGE_CURVE('',#6275,#6273,#203,.T.);
#8008=EDGE_CURVE('',#6276,#6274,#204,.T.);
#8009=EDGE_CURVE('',#6277,#6278,#3913,.T.);
#8010=EDGE_CURVE('',#6277,#6275,#205,.T.);
#8011=EDGE_CURVE('',#6278,#6276,#206,.T.);
#8012=EDGE_CURVE('',#6279,#6280,#3914,.T.);
#8013=EDGE_CURVE('',#6279,#6277,#207,.T.);
#8014=EDGE_CURVE('',#6280,#6278,#208,.T.);
#8015=EDGE_CURVE('',#6281,#6282,#3915,.T.);
#8016=EDGE_CURVE('',#6281,#6279,#209,.T.);
#8017=EDGE_CURVE('',#6282,#6280,#210,.T.);
#8018=EDGE_CURVE('',#6283,#6284,#3916,.T.);
#8019=EDGE_CURVE('',#6283,#6281,#211,.T.);
#8020=EDGE_CURVE('',#6284,#6282,#212,.T.);
#8021=EDGE_CURVE('',#6285,#6286,#3917,.T.);
#8022=EDGE_CURVE('',#6285,#6283,#213,.T.);
#8023=EDGE_CURVE('',#6286,#6284,#214,.T.);
#8024=EDGE_CURVE('',#6287,#6288,#3918,.T.);
#8025=EDGE_CURVE('',#6287,#6285,#215,.T.);
#8026=EDGE_CURVE('',#6288,#6286,#216,.T.);
#8027=EDGE_CURVE('',#6289,#6290,#3919,.T.);
#8028=EDGE_CURVE('',#6289,#6287,#217,.T.);
#8029=EDGE_CURVE('',#6290,#6288,#218,.T.);
#8030=EDGE_CURVE('',#6291,#6292,#3920,.T.);
#8031=EDGE_CURVE('',#6291,#6289,#219,.T.);
#8032=EDGE_CURVE('',#6292,#6290,#220,.T.);
#8033=EDGE_CURVE('',#6293,#6294,#3921,.T.);
#8034=EDGE_CURVE('',#6293,#6291,#221,.T.);
#8035=EDGE_CURVE('',#6294,#6292,#222,.T.);
#8036=EDGE_CURVE('',#6295,#6296,#3922,.T.);
#8037=EDGE_CURVE('',#6295,#6293,#223,.T.);
#8038=EDGE_CURVE('',#6296,#6294,#224,.T.);
#8039=EDGE_CURVE('',#6297,#6298,#3923,.T.);
#8040=EDGE_CURVE('',#6297,#6295,#225,.T.);
#8041=EDGE_CURVE('',#6298,#6296,#226,.T.);
#8042=EDGE_CURVE('',#6299,#6300,#3924,.T.);
#8043=EDGE_CURVE('',#6299,#6297,#227,.T.);
#8044=EDGE_CURVE('',#6300,#6298,#228,.T.);
#8045=EDGE_CURVE('',#6301,#6302,#3925,.T.);
#8046=EDGE_CURVE('',#6301,#6299,#229,.T.);
#8047=EDGE_CURVE('',#6302,#6300,#230,.T.);
#8048=EDGE_CURVE('',#6303,#6304,#3926,.T.);
#8049=EDGE_CURVE('',#6303,#6301,#231,.T.);
#8050=EDGE_CURVE('',#6304,#6302,#232,.T.);
#8051=EDGE_CURVE('',#6305,#6306,#3927,.T.);
#8052=EDGE_CURVE('',#6305,#6303,#233,.T.);
#8053=EDGE_CURVE('',#6306,#6304,#234,.T.);
#8054=EDGE_CURVE('',#6307,#6308,#3928,.T.);
#8055=EDGE_CURVE('',#6307,#6305,#235,.T.);
#8056=EDGE_CURVE('',#6308,#6306,#236,.T.);
#8057=EDGE_CURVE('',#6309,#6310,#3929,.T.);
#8058=EDGE_CURVE('',#6309,#6307,#237,.T.);
#8059=EDGE_CURVE('',#6310,#6308,#238,.T.);
#8060=EDGE_CURVE('',#6311,#6312,#3930,.T.);
#8061=EDGE_CURVE('',#6311,#6309,#239,.T.);
#8062=EDGE_CURVE('',#6312,#6310,#240,.T.);
#8063=EDGE_CURVE('',#6313,#6314,#3931,.T.);
#8064=EDGE_CURVE('',#6313,#6311,#241,.T.);
#8065=EDGE_CURVE('',#6314,#6312,#242,.T.);
#8066=EDGE_CURVE('',#6315,#6316,#3932,.T.);
#8067=EDGE_CURVE('',#6315,#6313,#243,.T.);
#8068=EDGE_CURVE('',#6316,#6314,#244,.T.);
#8069=EDGE_CURVE('',#6317,#6318,#3933,.T.);
#8070=EDGE_CURVE('',#6317,#6315,#245,.T.);
#8071=EDGE_CURVE('',#6318,#6316,#246,.T.);
#8072=EDGE_CURVE('',#6319,#6320,#3934,.T.);
#8073=EDGE_CURVE('',#6319,#6317,#247,.T.);
#8074=EDGE_CURVE('',#6320,#6318,#248,.T.);
#8075=EDGE_CURVE('',#6321,#6322,#3935,.T.);
#8076=EDGE_CURVE('',#6321,#6319,#249,.T.);
#8077=EDGE_CURVE('',#6322,#6320,#250,.T.);
#8078=EDGE_CURVE('',#6323,#6324,#1098,.T.);
#8079=EDGE_CURVE('',#6324,#6325,#3936,.T.);
#8080=EDGE_CURVE('',#6325,#6325,#1099,.T.);
#8081=EDGE_CURVE('',#6324,#6326,#1100,.T.);
#8082=EDGE_CURVE('',#6326,#6327,#1101,.T.);
#8083=EDGE_CURVE('',#6327,#6328,#1102,.T.);
#8084=EDGE_CURVE('',#6328,#6329,#1103,.T.);
#8085=EDGE_CURVE('',#6329,#6330,#1104,.T.);
#8086=EDGE_CURVE('',#6330,#6331,#1105,.T.);
#8087=EDGE_CURVE('',#6331,#6332,#1106,.T.);
#8088=EDGE_CURVE('',#6332,#6333,#1107,.T.);
#8089=EDGE_CURVE('',#6333,#6334,#1108,.T.);
#8090=EDGE_CURVE('',#6334,#6335,#1109,.T.);
#8091=EDGE_CURVE('',#6335,#6336,#1110,.T.);
#8092=EDGE_CURVE('',#6336,#6337,#1111,.T.);
#8093=EDGE_CURVE('',#6337,#6338,#1112,.T.);
#8094=EDGE_CURVE('',#6338,#6339,#1113,.T.);
#8095=EDGE_CURVE('',#6339,#6340,#1114,.T.);
#8096=EDGE_CURVE('',#6340,#6341,#1115,.T.);
#8097=EDGE_CURVE('',#6341,#6342,#1116,.T.);
#8098=EDGE_CURVE('',#6342,#6343,#1117,.T.);
#8099=EDGE_CURVE('',#6343,#6344,#1118,.T.);
#8100=EDGE_CURVE('',#6344,#6345,#1119,.T.);
#8101=EDGE_CURVE('',#6345,#6346,#1120,.T.);
#8102=EDGE_CURVE('',#6346,#6347,#1121,.T.);
#8103=EDGE_CURVE('',#6347,#6348,#1122,.T.);
#8104=EDGE_CURVE('',#6348,#6349,#1123,.T.);
#8105=EDGE_CURVE('',#6349,#6350,#1124,.T.);
#8106=EDGE_CURVE('',#6350,#6351,#1125,.T.);
#8107=EDGE_CURVE('',#6351,#6352,#1126,.T.);
#8108=EDGE_CURVE('',#6352,#6353,#1127,.T.);
#8109=EDGE_CURVE('',#6353,#6354,#1128,.T.);
#8110=EDGE_CURVE('',#6354,#6355,#1129,.T.);
#8111=EDGE_CURVE('',#6355,#6356,#1130,.T.);
#8112=EDGE_CURVE('',#6356,#6357,#1131,.T.);
#8113=EDGE_CURVE('',#6357,#6358,#1132,.T.);
#8114=EDGE_CURVE('',#6358,#6359,#1133,.T.);
#8115=EDGE_CURVE('',#6359,#6360,#1134,.T.);
#8116=EDGE_CURVE('',#6360,#6361,#1135,.T.);
#8117=EDGE_CURVE('',#6361,#6362,#1136,.T.);
#8118=EDGE_CURVE('',#6362,#6363,#1137,.T.);
#8119=EDGE_CURVE('',#6363,#6364,#1138,.T.);
#8120=EDGE_CURVE('',#6364,#6365,#1139,.T.);
#8121=EDGE_CURVE('',#6365,#6366,#1140,.T.);
#8122=EDGE_CURVE('',#6366,#6367,#1141,.T.);
#8123=EDGE_CURVE('',#6367,#6368,#1142,.T.);
#8124=EDGE_CURVE('',#6368,#6369,#1143,.T.);
#8125=EDGE_CURVE('',#6369,#6370,#1144,.T.);
#8126=EDGE_CURVE('',#6370,#6371,#1145,.T.);
#8127=EDGE_CURVE('',#6371,#6372,#1146,.T.);
#8128=EDGE_CURVE('',#6372,#6323,#1147,.T.);
#8129=EDGE_CURVE('',#6373,#6373,#1148,.T.);
#8130=EDGE_CURVE('',#6373,#6374,#3937,.T.);
#8131=EDGE_CURVE('',#6374,#6375,#1149,.T.);
#8132=EDGE_CURVE('',#6375,#6349,#3938,.T.);
#8133=EDGE_CURVE('',#6348,#6376,#3939,.T.);
#8134=EDGE_CURVE('',#6376,#6377,#1150,.T.);
#8135=EDGE_CURVE('',#6377,#6347,#3940,.T.);
#8136=EDGE_CURVE('',#6346,#6378,#3941,.T.);
#8137=EDGE_CURVE('',#6378,#6379,#1151,.T.);
#8138=EDGE_CURVE('',#6379,#6345,#3942,.T.);
#8139=EDGE_CURVE('',#6344,#6380,#3943,.T.);
#8140=EDGE_CURVE('',#6380,#6381,#1152,.T.);
#8141=EDGE_CURVE('',#6381,#6343,#3944,.T.);
#8142=EDGE_CURVE('',#6342,#6382,#3945,.T.);
#8143=EDGE_CURVE('',#6382,#6383,#1153,.T.);
#8144=EDGE_CURVE('',#6383,#6341,#3946,.T.);
#8145=EDGE_CURVE('',#6340,#6384,#3947,.T.);
#8146=EDGE_CURVE('',#6384,#6385,#1154,.T.);
#8147=EDGE_CURVE('',#6385,#6339,#3948,.T.);
#8148=EDGE_CURVE('',#6338,#6386,#3949,.T.);
#8149=EDGE_CURVE('',#6386,#6387,#1155,.T.);
#8150=EDGE_CURVE('',#6387,#6337,#3950,.T.);
#8151=EDGE_CURVE('',#6336,#6388,#3951,.T.);
#8152=EDGE_CURVE('',#6388,#6389,#1156,.T.);
#8153=EDGE_CURVE('',#6389,#6335,#3952,.T.);
#8154=EDGE_CURVE('',#6334,#6390,#3953,.T.);
#8155=EDGE_CURVE('',#6390,#6391,#1157,.T.);
#8156=EDGE_CURVE('',#6391,#6333,#3954,.T.);
#8157=EDGE_CURVE('',#6332,#6392,#3955,.T.);
#8158=EDGE_CURVE('',#6392,#6393,#1158,.T.);
#8159=EDGE_CURVE('',#6393,#6331,#3956,.T.);
#8160=EDGE_CURVE('',#6330,#6394,#3957,.T.);
#8161=EDGE_CURVE('',#6394,#6395,#1159,.T.);
#8162=EDGE_CURVE('',#6395,#6329,#3958,.T.);
#8163=EDGE_CURVE('',#6328,#6396,#3959,.T.);
#8164=EDGE_CURVE('',#6396,#6397,#1160,.T.);
#8165=EDGE_CURVE('',#6397,#6327,#3960,.T.);
#8166=EDGE_CURVE('',#6326,#6398,#3961,.T.);
#8167=EDGE_CURVE('',#6398,#6399,#1161,.T.);
#8168=EDGE_CURVE('',#6399,#6323,#3962,.T.);
#8169=EDGE_CURVE('',#6372,#6400,#3963,.T.);
#8170=EDGE_CURVE('',#6400,#6401,#1162,.T.);
#8171=EDGE_CURVE('',#6401,#6371,#3964,.T.);
#8172=EDGE_CURVE('',#6370,#6402,#3965,.T.);
#8173=EDGE_CURVE('',#6402,#6403,#1163,.T.);
#8174=EDGE_CURVE('',#6403,#6369,#3966,.T.);
#8175=EDGE_CURVE('',#6368,#6404,#3967,.T.);
#8176=EDGE_CURVE('',#6404,#6405,#1164,.T.);
#8177=EDGE_CURVE('',#6405,#6367,#3968,.T.);
#8178=EDGE_CURVE('',#6366,#6406,#3969,.T.);
#8179=EDGE_CURVE('',#6406,#6407,#1165,.T.);
#8180=EDGE_CURVE('',#6407,#6365,#3970,.T.);
#8181=EDGE_CURVE('',#6364,#6408,#3971,.T.);
#8182=EDGE_CURVE('',#6408,#6409,#1166,.T.);
#8183=EDGE_CURVE('',#6409,#6363,#3972,.T.);
#8184=EDGE_CURVE('',#6362,#6410,#3973,.T.);
#8185=EDGE_CURVE('',#6410,#6411,#1167,.T.);
#8186=EDGE_CURVE('',#6411,#6361,#3974,.T.);
#8187=EDGE_CURVE('',#6360,#6412,#3975,.T.);
#8188=EDGE_CURVE('',#6412,#6413,#1168,.T.);
#8189=EDGE_CURVE('',#6413,#6359,#3976,.T.);
#8190=EDGE_CURVE('',#6358,#6414,#3977,.T.);
#8191=EDGE_CURVE('',#6414,#6415,#1169,.T.);
#8192=EDGE_CURVE('',#6415,#6357,#3978,.T.);
#8193=EDGE_CURVE('',#6356,#6416,#3979,.T.);
#8194=EDGE_CURVE('',#6416,#6417,#1170,.T.);
#8195=EDGE_CURVE('',#6417,#6355,#3980,.T.);
#8196=EDGE_CURVE('',#6354,#6418,#3981,.T.);
#8197=EDGE_CURVE('',#6418,#6419,#1171,.T.);
#8198=EDGE_CURVE('',#6419,#6353,#3982,.T.);
#8199=EDGE_CURVE('',#6352,#6420,#3983,.T.);
#8200=EDGE_CURVE('',#6420,#6421,#1172,.T.);
#8201=EDGE_CURVE('',#6421,#6351,#3984,.T.);
#8202=EDGE_CURVE('',#6350,#6422,#3985,.T.);
#8203=EDGE_CURVE('',#6422,#6374,#1173,.T.);
#8204=EDGE_CURVE('',#6423,#6424,#1174,.T.);
#8205=EDGE_CURVE('',#6424,#6270,#251,.T.);
#8206=EDGE_CURVE('',#6269,#6423,#252,.T.);
#8207=EDGE_CURVE('',#6266,#6424,#253,.T.);
#8208=EDGE_CURVE('',#6425,#6212,#254,.T.);
#8209=EDGE_CURVE('',#6425,#6322,#255,.T.);
#8210=EDGE_CURVE('',#6212,#6426,#1175,.T.);
#8211=EDGE_CURVE('',#6426,#6211,#1176,.T.);
#8212=EDGE_CURVE('',#6211,#6427,#256,.T.);
#8213=EDGE_CURVE('',#6427,#6425,#1177,.T.);
#8214=EDGE_CURVE('',#6427,#6321,#257,.T.);
#8215=EDGE_CURVE('',#6423,#6265,#258,.T.);
#8216=EDGE_CURVE('',#6397,#6428,#3986,.T.);
#8217=EDGE_CURVE('',#6429,#6428,#3987,.T.);
#8218=EDGE_CURVE('',#6327,#6429,#3988,.T.);
#8219=EDGE_CURVE('',#6429,#6328,#3989,.T.);
#8220=EDGE_CURVE('',#6428,#6396,#3990,.T.);
#8221=EDGE_CURVE('',#6395,#6430,#3991,.T.);
#8222=EDGE_CURVE('',#6431,#6430,#3992,.T.);
#8223=EDGE_CURVE('',#6329,#6431,#3993,.T.);
#8224=EDGE_CURVE('',#6431,#6330,#3994,.T.);
#8225=EDGE_CURVE('',#6430,#6394,#3995,.T.);
#8226=EDGE_CURVE('',#6393,#6432,#3996,.T.);
#8227=EDGE_CURVE('',#6433,#6432,#3997,.T.);
#8228=EDGE_CURVE('',#6331,#6433,#3998,.T.);
#8229=EDGE_CURVE('',#6433,#6332,#3999,.T.);
#8230=EDGE_CURVE('',#6432,#6392,#4000,.T.);
#8231=EDGE_CURVE('',#6391,#6434,#4001,.T.);
#8232=EDGE_CURVE('',#6435,#6434,#4002,.T.);
#8233=EDGE_CURVE('',#6333,#6435,#4003,.T.);
#8234=EDGE_CURVE('',#6435,#6334,#4004,.T.);
#8235=EDGE_CURVE('',#6434,#6390,#4005,.T.);
#8236=EDGE_CURVE('',#6389,#6436,#4006,.T.);
#8237=EDGE_CURVE('',#6437,#6436,#4007,.T.);
#8238=EDGE_CURVE('',#6335,#6437,#4008,.T.);
#8239=EDGE_CURVE('',#6437,#6336,#4009,.T.);
#8240=EDGE_CURVE('',#6436,#6388,#4010,.T.);
#8241=EDGE_CURVE('',#6387,#6438,#4011,.T.);
#8242=EDGE_CURVE('',#6439,#6438,#4012,.T.);
#8243=EDGE_CURVE('',#6337,#6439,#4013,.T.);
#8244=EDGE_CURVE('',#6439,#6338,#4014,.T.);
#8245=EDGE_CURVE('',#6438,#6386,#4015,.T.);
#8246=EDGE_CURVE('',#6385,#6440,#4016,.T.);
#8247=EDGE_CURVE('',#6441,#6440,#4017,.T.);
#8248=EDGE_CURVE('',#6339,#6441,#4018,.T.);
#8249=EDGE_CURVE('',#6441,#6340,#4019,.T.);
#8250=EDGE_CURVE('',#6440,#6384,#4020,.T.);
#8251=EDGE_CURVE('',#6383,#6442,#4021,.T.);
#8252=EDGE_CURVE('',#6443,#6442,#4022,.T.);
#8253=EDGE_CURVE('',#6341,#6443,#4023,.T.);
#8254=EDGE_CURVE('',#6443,#6342,#4024,.T.);
#8255=EDGE_CURVE('',#6442,#6382,#4025,.T.);
#8256=EDGE_CURVE('',#6381,#6444,#4026,.T.);
#8257=EDGE_CURVE('',#6445,#6444,#4027,.T.);
#8258=EDGE_CURVE('',#6343,#6445,#4028,.T.);
#8259=EDGE_CURVE('',#6445,#6344,#4029,.T.);
#8260=EDGE_CURVE('',#6444,#6380,#4030,.T.);
#8261=EDGE_CURVE('',#6379,#6446,#4031,.T.);
#8262=EDGE_CURVE('',#6447,#6446,#4032,.T.);
#8263=EDGE_CURVE('',#6345,#6447,#4033,.T.);
#8264=EDGE_CURVE('',#6447,#6346,#4034,.T.);
#8265=EDGE_CURVE('',#6446,#6378,#4035,.T.);
#8266=EDGE_CURVE('',#6377,#6448,#4036,.T.);
#8267=EDGE_CURVE('',#6449,#6448,#4037,.T.);
#8268=EDGE_CURVE('',#6347,#6449,#4038,.T.);
#8269=EDGE_CURVE('',#6449,#6348,#4039,.T.);
#8270=EDGE_CURVE('',#6448,#6376,#4040,.T.);
#8271=EDGE_CURVE('',#6375,#6450,#4041,.T.);
#8272=EDGE_CURVE('',#6451,#6450,#4042,.T.);
#8273=EDGE_CURVE('',#6349,#6451,#4043,.T.);
#8274=EDGE_CURVE('',#6451,#6350,#4044,.T.);
#8275=EDGE_CURVE('',#6450,#6422,#4045,.T.);
#8276=EDGE_CURVE('',#6421,#6452,#4046,.T.);
#8277=EDGE_CURVE('',#6453,#6452,#4047,.T.);
#8278=EDGE_CURVE('',#6351,#6453,#4048,.T.);
#8279=EDGE_CURVE('',#6453,#6352,#4049,.T.);
#8280=EDGE_CURVE('',#6452,#6420,#4050,.T.);
#8281=EDGE_CURVE('',#6419,#6454,#4051,.T.);
#8282=EDGE_CURVE('',#6455,#6454,#4052,.T.);
#8283=EDGE_CURVE('',#6353,#6455,#4053,.T.);
#8284=EDGE_CURVE('',#6455,#6354,#4054,.T.);
#8285=EDGE_CURVE('',#6454,#6418,#4055,.T.);
#8286=EDGE_CURVE('',#6417,#6456,#4056,.T.);
#8287=EDGE_CURVE('',#6457,#6456,#4057,.T.);
#8288=EDGE_CURVE('',#6355,#6457,#4058,.T.);
#8289=EDGE_CURVE('',#6457,#6356,#4059,.T.);
#8290=EDGE_CURVE('',#6456,#6416,#4060,.T.);
#8291=EDGE_CURVE('',#6415,#6458,#4061,.T.);
#8292=EDGE_CURVE('',#6459,#6458,#4062,.T.);
#8293=EDGE_CURVE('',#6357,#6459,#4063,.T.);
#8294=EDGE_CURVE('',#6459,#6358,#4064,.T.);
#8295=EDGE_CURVE('',#6458,#6414,#4065,.T.);
#8296=EDGE_CURVE('',#6413,#6460,#4066,.T.);
#8297=EDGE_CURVE('',#6461,#6460,#4067,.T.);
#8298=EDGE_CURVE('',#6359,#6461,#4068,.T.);
#8299=EDGE_CURVE('',#6461,#6360,#4069,.T.);
#8300=EDGE_CURVE('',#6460,#6412,#4070,.T.);
#8301=EDGE_CURVE('',#6411,#6462,#4071,.T.);
#8302=EDGE_CURVE('',#6463,#6462,#4072,.T.);
#8303=EDGE_CURVE('',#6361,#6463,#4073,.T.);
#8304=EDGE_CURVE('',#6463,#6362,#4074,.T.);
#8305=EDGE_CURVE('',#6462,#6410,#4075,.T.);
#8306=EDGE_CURVE('',#6409,#6464,#4076,.T.);
#8307=EDGE_CURVE('',#6465,#6464,#4077,.T.);
#8308=EDGE_CURVE('',#6363,#6465,#4078,.T.);
#8309=EDGE_CURVE('',#6465,#6364,#4079,.T.);
#8310=EDGE_CURVE('',#6464,#6408,#4080,.T.);
#8311=EDGE_CURVE('',#6407,#6466,#4081,.T.);
#8312=EDGE_CURVE('',#6467,#6466,#4082,.T.);
#8313=EDGE_CURVE('',#6365,#6467,#4083,.T.);
#8314=EDGE_CURVE('',#6467,#6366,#4084,.T.);
#8315=EDGE_CURVE('',#6466,#6406,#4085,.T.);
#8316=EDGE_CURVE('',#6405,#6468,#4086,.T.);
#8317=EDGE_CURVE('',#6469,#6468,#4087,.T.);
#8318=EDGE_CURVE('',#6367,#6469,#4088,.T.);
#8319=EDGE_CURVE('',#6469,#6368,#4089,.T.);
#8320=EDGE_CURVE('',#6468,#6404,#4090,.T.);
#8321=EDGE_CURVE('',#6403,#6470,#4091,.T.);
#8322=EDGE_CURVE('',#6471,#6470,#4092,.T.);
#8323=EDGE_CURVE('',#6369,#6471,#4093,.T.);
#8324=EDGE_CURVE('',#6471,#6370,#4094,.T.);
#8325=EDGE_CURVE('',#6470,#6402,#4095,.T.);
#8326=EDGE_CURVE('',#6401,#6472,#4096,.T.);
#8327=EDGE_CURVE('',#6473,#6472,#4097,.T.);
#8328=EDGE_CURVE('',#6371,#6473,#4098,.T.);
#8329=EDGE_CURVE('',#6473,#6372,#4099,.T.);
#8330=EDGE_CURVE('',#6472,#6400,#4100,.T.);
#8331=EDGE_CURVE('',#6399,#6474,#4101,.T.);
#8332=EDGE_CURVE('',#6475,#6474,#4102,.T.);
#8333=EDGE_CURVE('',#6323,#6475,#4103,.T.);
#8334=EDGE_CURVE('',#6475,#6326,#4104,.T.);
#8335=EDGE_CURVE('',#6474,#6398,#4105,.T.);
#8336=EDGE_CURVE('',#6476,#6476,#1178,.T.);
#8337=EDGE_CURVE('',#6426,#6476,#4106,.T.);
#8338=EDGE_CURVE('',#6477,#6477,#1179,.T.);
#8339=EDGE_CURVE('',#6477,#6373,#4107,.T.);
#8340=EDGE_CURVE('',#6478,#6478,#1180,.T.);
#8341=EDGE_CURVE('',#6478,#6479,#4108,.T.);
#8342=EDGE_CURVE('',#6479,#6479,#1181,.T.);
#8343=EDGE_CURVE('',#6480,#6481,#1182,.T.);
#8344=EDGE_CURVE('',#6481,#6480,#1183,.T.);
#8345=EDGE_CURVE('',#6480,#6482,#4109,.T.);
#8346=EDGE_CURVE('',#6482,#6482,#1184,.T.);
#8347=EDGE_CURVE('',#6481,#6483,#4110,.T.);
#8348=EDGE_CURVE('',#6483,#6483,#1185,.T.);
#8349=EDGE_CURVE('',#6484,#6484,#1186,.T.);
#8350=EDGE_CURVE('',#6485,#6486,#3138,.T.);
#8351=EDGE_CURVE('',#6486,#6487,#4111,.T.);
#8352=EDGE_CURVE('',#6487,#6488,#4112,.F.);
#8353=EDGE_CURVE('',#6488,#6485,#4113,.T.);
#8354=EDGE_CURVE('',#6489,#6487,#1187,.T.);
#8355=EDGE_CURVE('',#6490,#6486,#1188,.T.);
#8356=EDGE_CURVE('',#6491,#6490,#259,.T.);
#8357=EDGE_CURVE('',#6492,#6491,#4114,.T.);
#8358=EDGE_CURVE('',#6492,#6493,#1189,.T.);
#8359=EDGE_CURVE('',#6494,#6493,#4115,.T.);
#8360=EDGE_CURVE('',#6495,#6494,#260,.T.);
#8361=EDGE_CURVE('',#6496,#6495,#1190,.T.);
#8362=EDGE_CURVE('',#6497,#6496,#4116,.T.);
#8363=EDGE_CURVE('',#6497,#6498,#1191,.T.);
#8364=EDGE_CURVE('',#6499,#6498,#4117,.T.);
#8365=EDGE_CURVE('',#6500,#6499,#1192,.T.);
#8366=EDGE_CURVE('',#6501,#6500,#4118,.T.);
#8367=EDGE_CURVE('',#6501,#6502,#1193,.T.);
#8368=EDGE_CURVE('',#6503,#6502,#4119,.T.);
#8369=EDGE_CURVE('',#6504,#6503,#1194,.T.);
#8370=EDGE_CURVE('',#6505,#6504,#4120,.T.);
#8371=EDGE_CURVE('',#6505,#6506,#1195,.T.);
#8372=EDGE_CURVE('',#6507,#6506,#4121,.T.);
#8373=EDGE_CURVE('',#6508,#6507,#1196,.T.);
#8374=EDGE_CURVE('',#6509,#6508,#4122,.T.);
#8375=EDGE_CURVE('',#6509,#6510,#1197,.T.);
#8376=EDGE_CURVE('',#6511,#6510,#4123,.T.);
#8377=EDGE_CURVE('',#6512,#6511,#1198,.T.);
#8378=EDGE_CURVE('',#6513,#6512,#4124,.T.);
#8379=EDGE_CURVE('',#6513,#6514,#1199,.T.);
#8380=EDGE_CURVE('',#6515,#6514,#4125,.T.);
#8381=EDGE_CURVE('',#6516,#6515,#1200,.T.);
#8382=EDGE_CURVE('',#6517,#6516,#4126,.T.);
#8383=EDGE_CURVE('',#6517,#6518,#1201,.T.);
#8384=EDGE_CURVE('',#6519,#6518,#4127,.T.);
#8385=EDGE_CURVE('',#6520,#6519,#1202,.T.);
#8386=EDGE_CURVE('',#6521,#6520,#4128,.T.);
#8387=EDGE_CURVE('',#6521,#6522,#1203,.T.);
#8388=EDGE_CURVE('',#6522,#6523,#4129,.T.);
#8389=EDGE_CURVE('',#6523,#6523,#1204,.T.);
#8390=EDGE_CURVE('',#6522,#6524,#1205,.T.);
#8391=EDGE_CURVE('',#6525,#6524,#4130,.T.);
#8392=EDGE_CURVE('',#6526,#6525,#1206,.T.);
#8393=EDGE_CURVE('',#6527,#6526,#4131,.T.);
#8394=EDGE_CURVE('',#6527,#6528,#1207,.T.);
#8395=EDGE_CURVE('',#6529,#6528,#4132,.T.);
#8396=EDGE_CURVE('',#6530,#6529,#1208,.T.);
#8397=EDGE_CURVE('',#6531,#6530,#4133,.T.);
#8398=EDGE_CURVE('',#6531,#6532,#1209,.T.);
#8399=EDGE_CURVE('',#6533,#6532,#4134,.T.);
#8400=EDGE_CURVE('',#6534,#6533,#1210,.T.);
#8401=EDGE_CURVE('',#6535,#6534,#4135,.T.);
#8402=EDGE_CURVE('',#6535,#6536,#1211,.T.);
#8403=EDGE_CURVE('',#6537,#6536,#4136,.T.);
#8404=EDGE_CURVE('',#6538,#6537,#1212,.T.);
#8405=EDGE_CURVE('',#6539,#6538,#4137,.T.);
#8406=EDGE_CURVE('',#6539,#6540,#1213,.T.);
#8407=EDGE_CURVE('',#6541,#6540,#4138,.T.);
#8408=EDGE_CURVE('',#6542,#6541,#1214,.T.);
#8409=EDGE_CURVE('',#6543,#6542,#4139,.T.);
#8410=EDGE_CURVE('',#6543,#6544,#1215,.T.);
#8411=EDGE_CURVE('',#6545,#6544,#4140,.T.);
#8412=EDGE_CURVE('',#6546,#6545,#1216,.T.);
#8413=EDGE_CURVE('',#6547,#6546,#4141,.T.);
#8414=EDGE_CURVE('',#6547,#6548,#1217,.T.);
#8415=EDGE_CURVE('',#6549,#6548,#4142,.T.);
#8416=EDGE_CURVE('',#6550,#6549,#1218,.T.);
#8417=EDGE_CURVE('',#6551,#6550,#4143,.T.);
#8418=EDGE_CURVE('',#6551,#6552,#1219,.T.);
#8419=EDGE_CURVE('',#6553,#6552,#4144,.T.);
#8420=EDGE_CURVE('',#6554,#6553,#1220,.T.);
#8421=EDGE_CURVE('',#6489,#6554,#4145,.T.);
#8422=EDGE_CURVE('',#6484,#6555,#4146,.T.);
#8423=EDGE_CURVE('',#6555,#6556,#261,.T.);
#8424=EDGE_CURVE('',#6520,#6556,#3139,.T.);
#8425=EDGE_CURVE('',#6557,#6519,#3140,.T.);
#8426=EDGE_CURVE('',#6557,#6558,#262,.T.);
#8427=EDGE_CURVE('',#6516,#6558,#3141,.T.);
#8428=EDGE_CURVE('',#6559,#6515,#3142,.T.);
#8429=EDGE_CURVE('',#6559,#6560,#263,.T.);
#8430=EDGE_CURVE('',#6512,#6560,#3143,.T.);
#8431=EDGE_CURVE('',#6561,#6511,#3144,.T.);
#8432=EDGE_CURVE('',#6561,#6562,#264,.T.);
#8433=EDGE_CURVE('',#6508,#6562,#3145,.T.);
#8434=EDGE_CURVE('',#6563,#6507,#3146,.T.);
#8435=EDGE_CURVE('',#6563,#6564,#265,.T.);
#8436=EDGE_CURVE('',#6504,#6564,#3147,.T.);
#8437=EDGE_CURVE('',#6565,#6503,#3148,.T.);
#8438=EDGE_CURVE('',#6565,#6566,#266,.T.);
#8439=EDGE_CURVE('',#6500,#6566,#3149,.T.);
#8440=EDGE_CURVE('',#6567,#6499,#3150,.T.);
#8441=EDGE_CURVE('',#6567,#6568,#267,.T.);
#8442=EDGE_CURVE('',#6496,#6568,#3151,.T.);
#8443=EDGE_CURVE('',#6490,#6495,#268,.T.);
#8444=EDGE_CURVE('',#6485,#6569,#269,.T.);
#8445=EDGE_CURVE('',#6554,#6569,#3152,.T.);
#8446=EDGE_CURVE('',#6570,#6553,#3153,.T.);
#8447=EDGE_CURVE('',#6570,#6571,#270,.T.);
#8448=EDGE_CURVE('',#6550,#6571,#3154,.T.);
#8449=EDGE_CURVE('',#6572,#6549,#3155,.T.);
#8450=EDGE_CURVE('',#6572,#6573,#271,.T.);
#8451=EDGE_CURVE('',#6546,#6573,#3156,.T.);
#8452=EDGE_CURVE('',#6574,#6545,#3157,.T.);
#8453=EDGE_CURVE('',#6574,#6575,#272,.T.);
#8454=EDGE_CURVE('',#6542,#6575,#3158,.T.);
#8455=EDGE_CURVE('',#6576,#6541,#3159,.T.);
#8456=EDGE_CURVE('',#6576,#6577,#273,.T.);
#8457=EDGE_CURVE('',#6538,#6577,#3160,.T.);
#8458=EDGE_CURVE('',#6578,#6537,#3161,.T.);
#8459=EDGE_CURVE('',#6578,#6579,#274,.T.);
#8460=EDGE_CURVE('',#6534,#6579,#3162,.T.);
#8461=EDGE_CURVE('',#6580,#6533,#3163,.T.);
#8462=EDGE_CURVE('',#6580,#6581,#275,.T.);
#8463=EDGE_CURVE('',#6530,#6581,#3164,.T.);
#8464=EDGE_CURVE('',#6582,#6529,#3165,.T.);
#8465=EDGE_CURVE('',#6582,#6583,#276,.T.);
#8466=EDGE_CURVE('',#6526,#6583,#3166,.T.);
#8467=EDGE_CURVE('',#6584,#6525,#3167,.T.);
#8468=EDGE_CURVE('',#6584,#6555,#277,.T.);
#8469=EDGE_CURVE('',#6569,#6585,#4147,.T.);
#8470=EDGE_CURVE('',#6585,#6489,#4148,.F.);
#8471=EDGE_CURVE('',#6552,#6586,#4149,.F.);
#8472=EDGE_CURVE('',#6586,#6570,#4150,.T.);
#8473=EDGE_CURVE('',#6571,#6587,#4151,.T.);
#8474=EDGE_CURVE('',#6587,#6551,#4152,.F.);
#8475=EDGE_CURVE('',#6548,#6588,#4153,.F.);
#8476=EDGE_CURVE('',#6588,#6572,#4154,.T.);
#8477=EDGE_CURVE('',#6573,#6589,#4155,.T.);
#8478=EDGE_CURVE('',#6589,#6547,#4156,.F.);
#8479=EDGE_CURVE('',#6544,#6590,#4157,.F.);
#8480=EDGE_CURVE('',#6590,#6574,#4158,.T.);
#8481=EDGE_CURVE('',#6575,#6591,#4159,.T.);
#8482=EDGE_CURVE('',#6591,#6543,#4160,.F.);
#8483=EDGE_CURVE('',#6540,#6592,#4161,.F.);
#8484=EDGE_CURVE('',#6592,#6576,#4162,.T.);
#8485=EDGE_CURVE('',#6577,#6593,#4163,.T.);
#8486=EDGE_CURVE('',#6593,#6539,#4164,.F.);
#8487=EDGE_CURVE('',#6536,#6594,#4165,.F.);
#8488=EDGE_CURVE('',#6594,#6578,#4166,.T.);
#8489=EDGE_CURVE('',#6579,#6595,#4167,.T.);
#8490=EDGE_CURVE('',#6595,#6535,#4168,.F.);
#8491=EDGE_CURVE('',#6532,#6596,#4169,.F.);
#8492=EDGE_CURVE('',#6596,#6580,#4170,.T.);
#8493=EDGE_CURVE('',#6581,#6597,#4171,.T.);
#8494=EDGE_CURVE('',#6597,#6531,#4172,.F.);
#8495=EDGE_CURVE('',#6528,#6598,#4173,.F.);
#8496=EDGE_CURVE('',#6598,#6582,#4174,.T.);
#8497=EDGE_CURVE('',#6583,#6599,#4175,.T.);
#8498=EDGE_CURVE('',#6599,#6527,#4176,.F.);
#8499=EDGE_CURVE('',#6524,#6600,#4177,.F.);
#8500=EDGE_CURVE('',#6600,#6584,#4178,.T.);
#8501=EDGE_CURVE('',#6556,#6601,#4179,.T.);
#8502=EDGE_CURVE('',#6601,#6521,#4180,.F.);
#8503=EDGE_CURVE('',#6518,#6602,#4181,.F.);
#8504=EDGE_CURVE('',#6602,#6557,#4182,.T.);
#8505=EDGE_CURVE('',#6558,#6603,#4183,.T.);
#8506=EDGE_CURVE('',#6603,#6517,#4184,.F.);
#8507=EDGE_CURVE('',#6514,#6604,#4185,.F.);
#8508=EDGE_CURVE('',#6604,#6559,#4186,.T.);
#8509=EDGE_CURVE('',#6560,#6605,#4187,.T.);
#8510=EDGE_CURVE('',#6605,#6513,#4188,.F.);
#8511=EDGE_CURVE('',#6510,#6606,#4189,.F.);
#8512=EDGE_CURVE('',#6606,#6561,#4190,.T.);
#8513=EDGE_CURVE('',#6562,#6607,#4191,.T.);
#8514=EDGE_CURVE('',#6607,#6509,#4192,.F.);
#8515=EDGE_CURVE('',#6506,#6608,#4193,.F.);
#8516=EDGE_CURVE('',#6608,#6563,#4194,.T.);
#8517=EDGE_CURVE('',#6564,#6609,#4195,.T.);
#8518=EDGE_CURVE('',#6609,#6505,#4196,.F.);
#8519=EDGE_CURVE('',#6502,#6610,#4197,.F.);
#8520=EDGE_CURVE('',#6610,#6565,#4198,.T.);
#8521=EDGE_CURVE('',#6566,#6611,#4199,.T.);
#8522=EDGE_CURVE('',#6611,#6501,#4200,.F.);
#8523=EDGE_CURVE('',#6498,#6612,#4201,.F.);
#8524=EDGE_CURVE('',#6612,#6567,#4202,.T.);
#8525=EDGE_CURVE('',#6568,#6613,#4203,.T.);
#8526=EDGE_CURVE('',#6613,#6497,#4204,.F.);
#8527=EDGE_CURVE('',#6614,#6615,#278,.T.);
#8528=EDGE_CURVE('',#6615,#6491,#279,.T.);
#8529=EDGE_CURVE('',#6494,#6614,#280,.T.);
#8530=EDGE_CURVE('',#6615,#6616,#4205,.T.);
#8531=EDGE_CURVE('',#6616,#6492,#4206,.F.);
#8532=EDGE_CURVE('',#6493,#6617,#4207,.F.);
#8533=EDGE_CURVE('',#6617,#6614,#4208,.T.);
#8534=EDGE_CURVE('',#6616,#6617,#1221,.T.);
#8535=EDGE_CURVE('',#6483,#6618,#4209,.T.);
#8536=EDGE_CURVE('',#6618,#6618,#1222,.T.);
#8537=EDGE_CURVE('',#6619,#6620,#4210,.T.);
#8538=EDGE_CURVE('',#6621,#6619,#4211,.T.);
#8539=EDGE_CURVE('',#6622,#6621,#4212,.T.);
#8540=EDGE_CURVE('',#6623,#6622,#4213,.T.);
#8541=EDGE_CURVE('',#6624,#6623,#4214,.T.);
#8542=EDGE_CURVE('',#6620,#6624,#4215,.T.);
#8543=EDGE_CURVE('',#6625,#6626,#4216,.T.);
#8544=EDGE_CURVE('',#6626,#6627,#4217,.T.);
#8545=EDGE_CURVE('',#6627,#6628,#4218,.T.);
#8546=EDGE_CURVE('',#6625,#6628,#4219,.T.);
#8547=EDGE_CURVE('',#6626,#6629,#4220,.T.);
#8548=EDGE_CURVE('',#6629,#6630,#4221,.T.);
#8549=EDGE_CURVE('',#6630,#6627,#4222,.T.);
#8550=EDGE_CURVE('',#6631,#6632,#4223,.T.);
#8551=EDGE_CURVE('',#6632,#6633,#4224,.T.);
#8552=EDGE_CURVE('',#6633,#6634,#4225,.T.);
#8553=EDGE_CURVE('',#6634,#6631,#4226,.T.);
#8554=EDGE_CURVE('',#6635,#6633,#4227,.T.);
#8555=EDGE_CURVE('',#6632,#6636,#4228,.T.);
#8556=EDGE_CURVE('',#6636,#6635,#4229,.T.);
#8557=EDGE_CURVE('',#6629,#6631,#4230,.T.);
#8558=EDGE_CURVE('',#6634,#6630,#4231,.T.);
#8559=EDGE_CURVE('',#6628,#6635,#4232,.T.);
#8560=EDGE_CURVE('',#6636,#6625,#4233,.T.);
#8561=EDGE_CURVE('',#6630,#6620,#4234,.T.);
#8562=EDGE_CURVE('',#6627,#6624,#4235,.T.);
#8563=EDGE_CURVE('',#6634,#6619,#4236,.T.);
#8564=EDGE_CURVE('',#6633,#6621,#4237,.T.);
#8565=EDGE_CURVE('',#6637,#6637,#1223,.T.);
#8566=EDGE_CURVE('',#6635,#6622,#4238,.T.);
#8567=EDGE_CURVE('',#6628,#6623,#4239,.T.);
#8568=EDGE_CURVE('',#6613,#6612,#1224,.T.);
#8569=EDGE_CURVE('',#6611,#6610,#1225,.T.);
#8570=EDGE_CURVE('',#6609,#6608,#1226,.T.);
#8571=EDGE_CURVE('',#6607,#6606,#1227,.T.);
#8572=EDGE_CURVE('',#6605,#6604,#1228,.T.);
#8573=EDGE_CURVE('',#6603,#6602,#1229,.T.);
#8574=EDGE_CURVE('',#6601,#6600,#1230,.T.);
#8575=EDGE_CURVE('',#6599,#6598,#1231,.T.);
#8576=EDGE_CURVE('',#6597,#6596,#1232,.T.);
#8577=EDGE_CURVE('',#6595,#6594,#1233,.T.);
#8578=EDGE_CURVE('',#6593,#6592,#1234,.T.);
#8579=EDGE_CURVE('',#6591,#6590,#1235,.T.);
#8580=EDGE_CURVE('',#6589,#6588,#1236,.T.);
#8581=EDGE_CURVE('',#6587,#6586,#1237,.T.);
#8582=EDGE_CURVE('',#6585,#6488,#1238,.T.);
#8583=EDGE_CURVE('',#6523,#6637,#4240,.T.);
#8584=EDGE_CURVE('',#6638,#6639,#4241,.T.);
#8585=EDGE_CURVE('',#6638,#6640,#281,.T.);
#8586=EDGE_CURVE('',#6640,#6641,#1239,.T.);
#8587=EDGE_CURVE('',#6641,#6639,#282,.T.);
#8588=EDGE_CURVE('',#6642,#6643,#4242,.T.);
#8589=EDGE_CURVE('',#6642,#6638,#283,.T.);
#8590=EDGE_CURVE('',#6639,#6643,#284,.T.);
#8591=EDGE_CURVE('',#6644,#6645,#4243,.T.);
#8592=EDGE_CURVE('',#6644,#6642,#285,.T.);
#8593=EDGE_CURVE('',#6643,#6645,#286,.T.);
#8594=EDGE_CURVE('',#6646,#6647,#4244,.T.);
#8595=EDGE_CURVE('',#6646,#6644,#287,.T.);
#8596=EDGE_CURVE('',#6645,#6647,#288,.T.);
#8597=EDGE_CURVE('',#6648,#6649,#4245,.T.);
#8598=EDGE_CURVE('',#6648,#6646,#289,.T.);
#8599=EDGE_CURVE('',#6647,#6649,#290,.T.);
#8600=EDGE_CURVE('',#6650,#6651,#4246,.T.);
#8601=EDGE_CURVE('',#6650,#6648,#291,.T.);
#8602=EDGE_CURVE('',#6649,#6651,#292,.T.);
#8603=EDGE_CURVE('',#6652,#6653,#4247,.T.);
#8604=EDGE_CURVE('',#6652,#6650,#293,.T.);
#8605=EDGE_CURVE('',#6651,#6653,#294,.T.);
#8606=EDGE_CURVE('',#6654,#6655,#4248,.T.);
#8607=EDGE_CURVE('',#6654,#6652,#295,.T.);
#8608=EDGE_CURVE('',#6653,#6655,#296,.T.);
#8609=EDGE_CURVE('',#6656,#6657,#4249,.T.);
#8610=EDGE_CURVE('',#6656,#6654,#297,.T.);
#8611=EDGE_CURVE('',#6655,#6657,#298,.T.);
#8612=EDGE_CURVE('',#6658,#6659,#4250,.T.);
#8613=EDGE_CURVE('',#6658,#6656,#299,.T.);
#8614=EDGE_CURVE('',#6657,#6659,#300,.T.);
#8615=EDGE_CURVE('',#6660,#6661,#4251,.T.);
#8616=EDGE_CURVE('',#6660,#6658,#301,.T.);
#8617=EDGE_CURVE('',#6659,#6661,#302,.T.);
#8618=EDGE_CURVE('',#6662,#6663,#4252,.T.);
#8619=EDGE_CURVE('',#6662,#6660,#303,.T.);
#8620=EDGE_CURVE('',#6661,#6663,#304,.T.);
#8621=EDGE_CURVE('',#6664,#6665,#4253,.T.);
#8622=EDGE_CURVE('',#6664,#6662,#305,.T.);
#8623=EDGE_CURVE('',#6663,#6665,#306,.T.);
#8624=EDGE_CURVE('',#6666,#6667,#4254,.T.);
#8625=EDGE_CURVE('',#6666,#6664,#307,.T.);
#8626=EDGE_CURVE('',#6665,#6667,#308,.T.);
#8627=EDGE_CURVE('',#6668,#6669,#4255,.T.);
#8628=EDGE_CURVE('',#6668,#6666,#309,.T.);
#8629=EDGE_CURVE('',#6667,#6669,#310,.T.);
#8630=EDGE_CURVE('',#6670,#6671,#4256,.T.);
#8631=EDGE_CURVE('',#6670,#6668,#311,.T.);
#8632=EDGE_CURVE('',#6669,#6671,#312,.T.);
#8633=EDGE_CURVE('',#6672,#6673,#4257,.T.);
#8634=EDGE_CURVE('',#6672,#6670,#313,.T.);
#8635=EDGE_CURVE('',#6671,#6673,#314,.T.);
#8636=EDGE_CURVE('',#6674,#6675,#4258,.T.);
#8637=EDGE_CURVE('',#6674,#6672,#315,.T.);
#8638=EDGE_CURVE('',#6673,#6675,#316,.T.);
#8639=EDGE_CURVE('',#6676,#6677,#4259,.T.);
#8640=EDGE_CURVE('',#6676,#6674,#317,.T.);
#8641=EDGE_CURVE('',#6675,#6677,#318,.T.);
#8642=EDGE_CURVE('',#6678,#6679,#4260,.T.);
#8643=EDGE_CURVE('',#6678,#6676,#319,.T.);
#8644=EDGE_CURVE('',#6677,#6679,#320,.T.);
#8645=EDGE_CURVE('',#6680,#6681,#4261,.T.);
#8646=EDGE_CURVE('',#6680,#6678,#321,.T.);
#8647=EDGE_CURVE('',#6679,#6681,#322,.T.);
#8648=EDGE_CURVE('',#6682,#6683,#4262,.T.);
#8649=EDGE_CURVE('',#6682,#6680,#323,.T.);
#8650=EDGE_CURVE('',#6681,#6683,#324,.T.);
#8651=EDGE_CURVE('',#6684,#6685,#4263,.T.);
#8652=EDGE_CURVE('',#6684,#6682,#325,.T.);
#8653=EDGE_CURVE('',#6683,#6685,#326,.T.);
#8654=EDGE_CURVE('',#6686,#6687,#4264,.T.);
#8655=EDGE_CURVE('',#6686,#6688,#327,.T.);
#8656=EDGE_CURVE('',#6689,#6688,#1240,.T.);
#8657=EDGE_CURVE('',#6687,#6689,#328,.T.);
#8658=EDGE_CURVE('',#6690,#6691,#4265,.T.);
#8659=EDGE_CURVE('',#6690,#6686,#329,.T.);
#8660=EDGE_CURVE('',#6691,#6687,#330,.T.);
#8661=EDGE_CURVE('',#6692,#6693,#4266,.T.);
#8662=EDGE_CURVE('',#6692,#6690,#331,.T.);
#8663=EDGE_CURVE('',#6693,#6691,#332,.T.);
#8664=EDGE_CURVE('',#6694,#6695,#4267,.T.);
#8665=EDGE_CURVE('',#6694,#6692,#333,.T.);
#8666=EDGE_CURVE('',#6695,#6693,#334,.T.);
#8667=EDGE_CURVE('',#6696,#6697,#4268,.T.);
#8668=EDGE_CURVE('',#6696,#6694,#335,.T.);
#8669=EDGE_CURVE('',#6697,#6695,#336,.T.);
#8670=EDGE_CURVE('',#6698,#6699,#4269,.T.);
#8671=EDGE_CURVE('',#6698,#6696,#337,.T.);
#8672=EDGE_CURVE('',#6699,#6697,#338,.T.);
#8673=EDGE_CURVE('',#6700,#6701,#4270,.T.);
#8674=EDGE_CURVE('',#6700,#6698,#339,.T.);
#8675=EDGE_CURVE('',#6701,#6699,#340,.T.);
#8676=EDGE_CURVE('',#6702,#6703,#4271,.T.);
#8677=EDGE_CURVE('',#6702,#6700,#341,.T.);
#8678=EDGE_CURVE('',#6703,#6701,#342,.T.);
#8679=EDGE_CURVE('',#6704,#6705,#4272,.T.);
#8680=EDGE_CURVE('',#6704,#6702,#343,.T.);
#8681=EDGE_CURVE('',#6705,#6703,#344,.T.);
#8682=EDGE_CURVE('',#6706,#6707,#4273,.T.);
#8683=EDGE_CURVE('',#6706,#6704,#345,.T.);
#8684=EDGE_CURVE('',#6707,#6705,#346,.T.);
#8685=EDGE_CURVE('',#6708,#6709,#4274,.T.);
#8686=EDGE_CURVE('',#6708,#6706,#347,.T.);
#8687=EDGE_CURVE('',#6709,#6707,#348,.T.);
#8688=EDGE_CURVE('',#6710,#6711,#4275,.T.);
#8689=EDGE_CURVE('',#6710,#6708,#349,.T.);
#8690=EDGE_CURVE('',#6711,#6709,#350,.T.);
#8691=EDGE_CURVE('',#6712,#6713,#4276,.T.);
#8692=EDGE_CURVE('',#6712,#6710,#351,.T.);
#8693=EDGE_CURVE('',#6713,#6711,#352,.T.);
#8694=EDGE_CURVE('',#6714,#6715,#4277,.T.);
#8695=EDGE_CURVE('',#6714,#6712,#353,.T.);
#8696=EDGE_CURVE('',#6715,#6713,#354,.T.);
#8697=EDGE_CURVE('',#6716,#6717,#4278,.T.);
#8698=EDGE_CURVE('',#6716,#6714,#355,.T.);
#8699=EDGE_CURVE('',#6717,#6715,#356,.T.);
#8700=EDGE_CURVE('',#6718,#6719,#4279,.T.);
#8701=EDGE_CURVE('',#6718,#6716,#357,.T.);
#8702=EDGE_CURVE('',#6719,#6717,#358,.T.);
#8703=EDGE_CURVE('',#6720,#6721,#4280,.T.);
#8704=EDGE_CURVE('',#6720,#6718,#359,.T.);
#8705=EDGE_CURVE('',#6721,#6719,#360,.T.);
#8706=EDGE_CURVE('',#6722,#6723,#4281,.T.);
#8707=EDGE_CURVE('',#6722,#6720,#361,.T.);
#8708=EDGE_CURVE('',#6723,#6721,#362,.T.);
#8709=EDGE_CURVE('',#6724,#6725,#4282,.T.);
#8710=EDGE_CURVE('',#6724,#6722,#363,.T.);
#8711=EDGE_CURVE('',#6725,#6723,#364,.T.);
#8712=EDGE_CURVE('',#6726,#6727,#4283,.T.);
#8713=EDGE_CURVE('',#6726,#6724,#365,.T.);
#8714=EDGE_CURVE('',#6727,#6725,#366,.T.);
#8715=EDGE_CURVE('',#6728,#6729,#4284,.T.);
#8716=EDGE_CURVE('',#6728,#6726,#367,.T.);
#8717=EDGE_CURVE('',#6729,#6727,#368,.T.);
#8718=EDGE_CURVE('',#6730,#6731,#4285,.T.);
#8719=EDGE_CURVE('',#6730,#6728,#369,.T.);
#8720=EDGE_CURVE('',#6731,#6729,#370,.T.);
#8721=EDGE_CURVE('',#6732,#6689,#371,.T.);
#8722=EDGE_CURVE('',#6685,#6732,#372,.T.);
#8723=EDGE_CURVE('',#6733,#6641,#373,.T.);
#8724=EDGE_CURVE('',#6733,#6731,#374,.T.);
#8725=EDGE_CURVE('',#6641,#6734,#1241,.T.);
#8726=EDGE_CURVE('',#6734,#6640,#1242,.T.);
#8727=EDGE_CURVE('',#6640,#6735,#375,.T.);
#8728=EDGE_CURVE('',#6735,#6733,#1243,.T.);
#8729=EDGE_CURVE('',#6735,#6730,#376,.T.);
#8730=EDGE_CURVE('',#6688,#6736,#377,.T.);
#8731=EDGE_CURVE('',#6736,#6684,#378,.T.);
#8732=EDGE_CURVE('',#6736,#6732,#1244,.F.);
#8733=EDGE_CURVE('',#6737,#6737,#1245,.T.);
#8734=EDGE_CURVE('',#6734,#6737,#4286,.T.);
#8735=EDGE_CURVE('',#6738,#6739,#3168,.T.);
#8736=EDGE_CURVE('',#6740,#6738,#3169,.T.);
#8737=EDGE_CURVE('',#6741,#6740,#3170,.T.);
#8738=EDGE_CURVE('',#6742,#6741,#3171,.T.);
#8739=EDGE_CURVE('',#6743,#6742,#3172,.T.);
#8740=EDGE_CURVE('',#6743,#6744,#4287,.T.);
#8741=EDGE_CURVE('',#6744,#6744,#1246,.T.);
#8742=EDGE_CURVE('',#6745,#6743,#3173,.T.);
#8743=EDGE_CURVE('',#6739,#6745,#3174,.T.);
#8744=EDGE_CURVE('',#6746,#6741,#4288,.T.);
#8745=EDGE_CURVE('',#6746,#6747,#4289,.T.);
#8746=EDGE_CURVE('',#6747,#6742,#4290,.T.);
#8747=EDGE_CURVE('',#6748,#6740,#4291,.T.);
#8748=EDGE_CURVE('',#6748,#6746,#4292,.T.);
#8749=EDGE_CURVE('',#6749,#6738,#4293,.T.);
#8750=EDGE_CURVE('',#6749,#6748,#4294,.T.);
#8751=EDGE_CURVE('',#6750,#6739,#4295,.T.);
#8752=EDGE_CURVE('',#6750,#6749,#4296,.T.);
#8753=EDGE_CURVE('',#6751,#6745,#4297,.T.);
#8754=EDGE_CURVE('',#6751,#6750,#4298,.T.);
#8755=EDGE_CURVE('',#6747,#6751,#4299,.T.);
#8756=EDGE_CURVE('',#6752,#6753,#4300,.T.);
#8757=EDGE_CURVE('',#6752,#6754,#379,.T.);
#8758=EDGE_CURVE('',#6754,#6755,#1247,.T.);
#8759=EDGE_CURVE('',#6755,#6753,#380,.T.);
#8760=EDGE_CURVE('',#6756,#6757,#4301,.T.);
#8761=EDGE_CURVE('',#6756,#6752,#381,.T.);
#8762=EDGE_CURVE('',#6753,#6757,#382,.T.);
#8763=EDGE_CURVE('',#6758,#6759,#4302,.T.);
#8764=EDGE_CURVE('',#6758,#6756,#383,.T.);
#8765=EDGE_CURVE('',#6757,#6759,#384,.T.);
#8766=EDGE_CURVE('',#6760,#6761,#4303,.T.);
#8767=EDGE_CURVE('',#6760,#6758,#385,.T.);
#8768=EDGE_CURVE('',#6759,#6761,#386,.T.);
#8769=EDGE_CURVE('',#6762,#6763,#4304,.T.);
#8770=EDGE_CURVE('',#6762,#6760,#387,.T.);
#8771=EDGE_CURVE('',#6761,#6763,#388,.T.);
#8772=EDGE_CURVE('',#6764,#6765,#4305,.T.);
#8773=EDGE_CURVE('',#6764,#6762,#389,.T.);
#8774=EDGE_CURVE('',#6763,#6765,#390,.T.);
#8775=EDGE_CURVE('',#6766,#6767,#4306,.T.);
#8776=EDGE_CURVE('',#6766,#6764,#391,.T.);
#8777=EDGE_CURVE('',#6765,#6767,#392,.T.);
#8778=EDGE_CURVE('',#6768,#6769,#4307,.T.);
#8779=EDGE_CURVE('',#6768,#6766,#393,.T.);
#8780=EDGE_CURVE('',#6767,#6769,#394,.T.);
#8781=EDGE_CURVE('',#6770,#6771,#4308,.T.);
#8782=EDGE_CURVE('',#6770,#6768,#395,.T.);
#8783=EDGE_CURVE('',#6769,#6771,#396,.T.);
#8784=EDGE_CURVE('',#6772,#6773,#4309,.T.);
#8785=EDGE_CURVE('',#6772,#6770,#397,.T.);
#8786=EDGE_CURVE('',#6771,#6773,#398,.T.);
#8787=EDGE_CURVE('',#6774,#6775,#4310,.T.);
#8788=EDGE_CURVE('',#6774,#6772,#399,.T.);
#8789=EDGE_CURVE('',#6773,#6775,#400,.T.);
#8790=EDGE_CURVE('',#6776,#6777,#4311,.T.);
#8791=EDGE_CURVE('',#6776,#6774,#401,.T.);
#8792=EDGE_CURVE('',#6775,#6777,#402,.T.);
#8793=EDGE_CURVE('',#6778,#6779,#4312,.T.);
#8794=EDGE_CURVE('',#6778,#6776,#403,.T.);
#8795=EDGE_CURVE('',#6777,#6779,#404,.T.);
#8796=EDGE_CURVE('',#6780,#6781,#4313,.T.);
#8797=EDGE_CURVE('',#6780,#6778,#405,.T.);
#8798=EDGE_CURVE('',#6779,#6781,#406,.T.);
#8799=EDGE_CURVE('',#6782,#6783,#4314,.T.);
#8800=EDGE_CURVE('',#6782,#6780,#407,.T.);
#8801=EDGE_CURVE('',#6781,#6783,#408,.T.);
#8802=EDGE_CURVE('',#6784,#6785,#4315,.T.);
#8803=EDGE_CURVE('',#6784,#6782,#409,.T.);
#8804=EDGE_CURVE('',#6783,#6785,#410,.T.);
#8805=EDGE_CURVE('',#6786,#6787,#4316,.T.);
#8806=EDGE_CURVE('',#6786,#6784,#411,.T.);
#8807=EDGE_CURVE('',#6785,#6787,#412,.T.);
#8808=EDGE_CURVE('',#6788,#6789,#4317,.T.);
#8809=EDGE_CURVE('',#6788,#6786,#413,.T.);
#8810=EDGE_CURVE('',#6787,#6789,#414,.T.);
#8811=EDGE_CURVE('',#6790,#6791,#4318,.T.);
#8812=EDGE_CURVE('',#6790,#6788,#415,.T.);
#8813=EDGE_CURVE('',#6789,#6791,#416,.T.);
#8814=EDGE_CURVE('',#6792,#6793,#4319,.T.);
#8815=EDGE_CURVE('',#6792,#6790,#417,.T.);
#8816=EDGE_CURVE('',#6791,#6793,#418,.T.);
#8817=EDGE_CURVE('',#6794,#6795,#4320,.T.);
#8818=EDGE_CURVE('',#6794,#6792,#419,.T.);
#8819=EDGE_CURVE('',#6793,#6795,#420,.T.);
#8820=EDGE_CURVE('',#6796,#6797,#4321,.T.);
#8821=EDGE_CURVE('',#6796,#6794,#421,.T.);
#8822=EDGE_CURVE('',#6795,#6797,#422,.T.);
#8823=EDGE_CURVE('',#6798,#6799,#4322,.T.);
#8824=EDGE_CURVE('',#6798,#6796,#423,.T.);
#8825=EDGE_CURVE('',#6797,#6799,#424,.T.);
#8826=EDGE_CURVE('',#6800,#6801,#4323,.T.);
#8827=EDGE_CURVE('',#6800,#6798,#425,.T.);
#8828=EDGE_CURVE('',#6799,#6801,#426,.T.);
#8829=EDGE_CURVE('',#6802,#6803,#4324,.T.);
#8830=EDGE_CURVE('',#6802,#6800,#427,.T.);
#8831=EDGE_CURVE('',#6801,#6803,#428,.T.);
#8832=EDGE_CURVE('',#6804,#6805,#4325,.T.);
#8833=EDGE_CURVE('',#6804,#6802,#429,.T.);
#8834=EDGE_CURVE('',#6803,#6805,#430,.T.);
#8835=EDGE_CURVE('',#6806,#6807,#4326,.T.);
#8836=EDGE_CURVE('',#6806,#6804,#431,.T.);
#8837=EDGE_CURVE('',#6805,#6807,#432,.T.);
#8838=EDGE_CURVE('',#6808,#6809,#4327,.T.);
#8839=EDGE_CURVE('',#6808,#6806,#433,.T.);
#8840=EDGE_CURVE('',#6807,#6809,#434,.T.);
#8841=EDGE_CURVE('',#6810,#6811,#4328,.T.);
#8842=EDGE_CURVE('',#6810,#6812,#435,.T.);
#8843=EDGE_CURVE('',#6813,#6812,#1248,.T.);
#8844=EDGE_CURVE('',#6811,#6813,#436,.T.);
#8845=EDGE_CURVE('',#6814,#6815,#4329,.T.);
#8846=EDGE_CURVE('',#6814,#6810,#437,.T.);
#8847=EDGE_CURVE('',#6815,#6811,#438,.T.);
#8848=EDGE_CURVE('',#6816,#6817,#4330,.T.);
#8849=EDGE_CURVE('',#6816,#6814,#439,.T.);
#8850=EDGE_CURVE('',#6817,#6815,#440,.T.);
#8851=EDGE_CURVE('',#6818,#6819,#4331,.T.);
#8852=EDGE_CURVE('',#6818,#6816,#441,.T.);
#8853=EDGE_CURVE('',#6819,#6817,#442,.T.);
#8854=EDGE_CURVE('',#6820,#6821,#4332,.T.);
#8855=EDGE_CURVE('',#6820,#6818,#443,.T.);
#8856=EDGE_CURVE('',#6821,#6819,#444,.T.);
#8857=EDGE_CURVE('',#6822,#6823,#4333,.T.);
#8858=EDGE_CURVE('',#6822,#6820,#445,.T.);
#8859=EDGE_CURVE('',#6823,#6821,#446,.T.);
#8860=EDGE_CURVE('',#6824,#6825,#4334,.T.);
#8861=EDGE_CURVE('',#6824,#6822,#447,.T.);
#8862=EDGE_CURVE('',#6825,#6823,#448,.T.);
#8863=EDGE_CURVE('',#6826,#6827,#4335,.T.);
#8864=EDGE_CURVE('',#6826,#6824,#449,.T.);
#8865=EDGE_CURVE('',#6827,#6825,#450,.T.);
#8866=EDGE_CURVE('',#6828,#6829,#4336,.T.);
#8867=EDGE_CURVE('',#6828,#6826,#451,.T.);
#8868=EDGE_CURVE('',#6829,#6827,#452,.T.);
#8869=EDGE_CURVE('',#6830,#6831,#4337,.T.);
#8870=EDGE_CURVE('',#6830,#6828,#453,.T.);
#8871=EDGE_CURVE('',#6831,#6829,#454,.T.);
#8872=EDGE_CURVE('',#6832,#6833,#4338,.T.);
#8873=EDGE_CURVE('',#6832,#6830,#455,.T.);
#8874=EDGE_CURVE('',#6833,#6831,#456,.T.);
#8875=EDGE_CURVE('',#6834,#6835,#4339,.T.);
#8876=EDGE_CURVE('',#6834,#6832,#457,.T.);
#8877=EDGE_CURVE('',#6835,#6833,#458,.T.);
#8878=EDGE_CURVE('',#6836,#6837,#4340,.T.);
#8879=EDGE_CURVE('',#6836,#6834,#459,.T.);
#8880=EDGE_CURVE('',#6837,#6835,#460,.T.);
#8881=EDGE_CURVE('',#6838,#6839,#4341,.T.);
#8882=EDGE_CURVE('',#6838,#6836,#461,.T.);
#8883=EDGE_CURVE('',#6839,#6837,#462,.T.);
#8884=EDGE_CURVE('',#6840,#6841,#4342,.T.);
#8885=EDGE_CURVE('',#6840,#6838,#463,.T.);
#8886=EDGE_CURVE('',#6841,#6839,#464,.T.);
#8887=EDGE_CURVE('',#6842,#6843,#4343,.T.);
#8888=EDGE_CURVE('',#6842,#6840,#465,.T.);
#8889=EDGE_CURVE('',#6843,#6841,#466,.T.);
#8890=EDGE_CURVE('',#6844,#6845,#4344,.T.);
#8891=EDGE_CURVE('',#6844,#6842,#467,.T.);
#8892=EDGE_CURVE('',#6845,#6843,#468,.T.);
#8893=EDGE_CURVE('',#6846,#6847,#4345,.T.);
#8894=EDGE_CURVE('',#6846,#6844,#469,.T.);
#8895=EDGE_CURVE('',#6847,#6845,#470,.T.);
#8896=EDGE_CURVE('',#6848,#6849,#4346,.T.);
#8897=EDGE_CURVE('',#6848,#6846,#471,.T.);
#8898=EDGE_CURVE('',#6849,#6847,#472,.T.);
#8899=EDGE_CURVE('',#6850,#6851,#4347,.T.);
#8900=EDGE_CURVE('',#6850,#6848,#473,.T.);
#8901=EDGE_CURVE('',#6851,#6849,#474,.T.);
#8902=EDGE_CURVE('',#6852,#6853,#4348,.T.);
#8903=EDGE_CURVE('',#6852,#6850,#475,.T.);
#8904=EDGE_CURVE('',#6853,#6851,#476,.T.);
#8905=EDGE_CURVE('',#6854,#6855,#4349,.T.);
#8906=EDGE_CURVE('',#6854,#6852,#477,.T.);
#8907=EDGE_CURVE('',#6855,#6853,#478,.T.);
#8908=EDGE_CURVE('',#6856,#6857,#4350,.T.);
#8909=EDGE_CURVE('',#6856,#6854,#479,.T.);
#8910=EDGE_CURVE('',#6857,#6855,#480,.T.);
#8911=EDGE_CURVE('',#6858,#6859,#4351,.T.);
#8912=EDGE_CURVE('',#6858,#6856,#481,.T.);
#8913=EDGE_CURVE('',#6859,#6857,#482,.T.);
#8914=EDGE_CURVE('',#6860,#6861,#4352,.T.);
#8915=EDGE_CURVE('',#6860,#6858,#483,.T.);
#8916=EDGE_CURVE('',#6861,#6859,#484,.T.);
#8917=EDGE_CURVE('',#6862,#6863,#4353,.T.);
#8918=EDGE_CURVE('',#6862,#6860,#485,.T.);
#8919=EDGE_CURVE('',#6863,#6861,#486,.T.);
#8920=EDGE_CURVE('',#6864,#6865,#4354,.T.);
#8921=EDGE_CURVE('',#6864,#6862,#487,.T.);
#8922=EDGE_CURVE('',#6865,#6863,#488,.T.);
#8923=EDGE_CURVE('',#6866,#6867,#4355,.T.);
#8924=EDGE_CURVE('',#6866,#6864,#489,.T.);
#8925=EDGE_CURVE('',#6867,#6865,#490,.T.);
#8926=EDGE_CURVE('',#6868,#6813,#491,.T.);
#8927=EDGE_CURVE('',#6809,#6868,#492,.T.);
#8928=EDGE_CURVE('',#6869,#6755,#493,.T.);
#8929=EDGE_CURVE('',#6869,#6867,#494,.T.);
#8930=EDGE_CURVE('',#6755,#6870,#1249,.T.);
#8931=EDGE_CURVE('',#6870,#6754,#1250,.T.);
#8932=EDGE_CURVE('',#6754,#6871,#495,.T.);
#8933=EDGE_CURVE('',#6871,#6869,#1251,.T.);
#8934=EDGE_CURVE('',#6871,#6866,#496,.T.);
#8935=EDGE_CURVE('',#6812,#6872,#497,.T.);
#8936=EDGE_CURVE('',#6872,#6808,#498,.T.);
#8937=EDGE_CURVE('',#6873,#6874,#4356,.T.);
#8938=EDGE_CURVE('',#6874,#6874,#1252,.T.);
#8939=EDGE_CURVE('',#6875,#6876,#499,.T.);
#8940=EDGE_CURVE('',#6875,#6877,#4357,.T.);
#8941=EDGE_CURVE('',#6877,#6878,#4358,.T.);
#8942=EDGE_CURVE('',#6876,#6878,#4359,.T.);
#8943=EDGE_CURVE('',#6876,#6879,#500,.T.);
#8944=EDGE_CURVE('',#6878,#6880,#4360,.T.);
#8945=EDGE_CURVE('',#6879,#6880,#4361,.T.);
#8946=EDGE_CURVE('',#6879,#6881,#501,.T.);
#8947=EDGE_CURVE('',#6880,#6882,#4362,.T.);
#8948=EDGE_CURVE('',#6881,#6882,#4363,.T.);
#8949=EDGE_CURVE('',#6881,#6883,#502,.T.);
#8950=EDGE_CURVE('',#6882,#6884,#4364,.T.);
#8951=EDGE_CURVE('',#6883,#6884,#4365,.T.);
#8952=EDGE_CURVE('',#6885,#6875,#503,.T.);
#8953=EDGE_CURVE('',#6885,#6886,#4366,.T.);
#8954=EDGE_CURVE('',#6886,#6877,#4367,.T.);
#8955=EDGE_CURVE('',#6883,#6885,#504,.T.);
#8956=EDGE_CURVE('',#6884,#6886,#4368,.T.);
#8957=EDGE_CURVE('',#6887,#6887,#1253,.T.);
#8958=EDGE_CURVE('',#6870,#6887,#4369,.T.);
#8959=EDGE_CURVE('',#6872,#6868,#1254,.T.);
#8960=EDGE_CURVE('',#6888,#6888,#1255,.T.);
#8961=EDGE_CURVE('',#6889,#6890,#1256,.T.);
#8962=EDGE_CURVE('',#6889,#6888,#4370,.T.);
#8963=EDGE_CURVE('',#6890,#6889,#1257,.T.);
#8964=EDGE_CURVE('',#6881,#6890,#3175,.T.);
#8965=EDGE_CURVE('',#6891,#6891,#1258,.T.);
#8966=EDGE_CURVE('',#6891,#6892,#4371,.T.);
#8967=EDGE_CURVE('',#6892,#6893,#1259,.T.);
#8968=EDGE_CURVE('',#6893,#6892,#1260,.T.);
#8969=EDGE_CURVE('',#6893,#6894,#4372,.T.);
#8970=EDGE_CURVE('',#6894,#6894,#1261,.T.);
#8971=EDGE_CURVE('',#6895,#6895,#1262,.T.);
#8972=EDGE_CURVE('',#6895,#6896,#4373,.T.);
#8973=EDGE_CURVE('',#6896,#6896,#1263,.T.);
#8974=EDGE_CURVE('',#6897,#6897,#1264,.T.);
#8975=EDGE_CURVE('',#6894,#6897,#4374,.T.);
#8976=EDGE_CURVE('',#6898,#6899,#3176,.T.);
#8977=EDGE_CURVE('',#6899,#6900,#4375,.T.);
#8978=EDGE_CURVE('',#6900,#6901,#3177,.T.);
#8979=EDGE_CURVE('',#6901,#6898,#4376,.T.);
#8980=EDGE_CURVE('',#6899,#6902,#3178,.T.);
#8981=EDGE_CURVE('',#6903,#6902,#4377,.T.);
#8982=EDGE_CURVE('',#6903,#6900,#3179,.T.);
#8983=EDGE_CURVE('',#6904,#6898,#3180,.T.);
#8984=EDGE_CURVE('',#6905,#6904,#3181,.T.);
#8985=EDGE_CURVE('',#6906,#6905,#3182,.T.);
#8986=EDGE_CURVE('',#6907,#6906,#3183,.T.);
#8987=EDGE_CURVE('',#6908,#6907,#3184,.T.);
#8988=EDGE_CURVE('',#6908,#6909,#4378,.T.);
#8989=EDGE_CURVE('',#6909,#6909,#1265,.T.);
#8990=EDGE_CURVE('',#6910,#6908,#3185,.T.);
#8991=EDGE_CURVE('',#6911,#6910,#3186,.T.);
#8992=EDGE_CURVE('',#6912,#6911,#3187,.T.);
#8993=EDGE_CURVE('',#6913,#6912,#3188,.T.);
#8994=EDGE_CURVE('',#6914,#6913,#3189,.T.);
#8995=EDGE_CURVE('',#6902,#6914,#3190,.T.);
#8996=EDGE_CURVE('',#6915,#6915,#1266,.T.);
#8997=EDGE_CURVE('',#6915,#6916,#4379,.T.);
#8998=EDGE_CURVE('',#6916,#6916,#1267,.T.);
#8999=EDGE_CURVE('',#6916,#6917,#4380,.T.);
#9000=EDGE_CURVE('',#6917,#6917,#1268,.T.);
#9001=EDGE_CURVE('',#6918,#6918,#1269,.T.);
#9002=EDGE_CURVE('',#6919,#6919,#1270,.T.);
#9003=EDGE_CURVE('',#6919,#6917,#4381,.T.);
#9004=EDGE_CURVE('',#6904,#6920,#4382,.T.);
#9005=EDGE_CURVE('',#6920,#6921,#3191,.T.);
#9006=EDGE_CURVE('',#6921,#6905,#4383,.T.);
#9007=EDGE_CURVE('',#6921,#6922,#3192,.T.);
#9008=EDGE_CURVE('',#6906,#6922,#4384,.T.);
#9009=EDGE_CURVE('',#6918,#6923,#4385,.T.);
#9010=EDGE_CURVE('',#6924,#6923,#3193,.T.);
#9011=EDGE_CURVE('',#6922,#6924,#3194,.T.);
#9012=EDGE_CURVE('',#6901,#6920,#3195,.T.);
#9013=EDGE_CURVE('',#6925,#6903,#3196,.T.);
#9014=EDGE_CURVE('',#6926,#6925,#3197,.T.);
#9015=EDGE_CURVE('',#6927,#6926,#3198,.T.);
#9016=EDGE_CURVE('',#6928,#6927,#3199,.T.);
#9017=EDGE_CURVE('',#6929,#6928,#3200,.T.);
#9018=EDGE_CURVE('',#6923,#6929,#3201,.T.);
#9019=EDGE_CURVE('',#6924,#6907,#4386,.T.);
#9020=EDGE_CURVE('',#6910,#6929,#4387,.T.);
#9021=EDGE_CURVE('',#6928,#6911,#4388,.T.);
#9022=EDGE_CURVE('',#6914,#6925,#4389,.T.);
#9023=EDGE_CURVE('',#6926,#6913,#4390,.T.);
#9024=EDGE_CURVE('',#6912,#6927,#4391,.T.);
#9025=EDGE_CURVE('',#6930,#6931,#4392,.T.);
#9026=EDGE_CURVE('',#6930,#6932,#505,.T.);
#9027=EDGE_CURVE('',#6932,#6933,#1271,.T.);
#9028=EDGE_CURVE('',#6933,#6931,#506,.T.);
#9029=EDGE_CURVE('',#6934,#6935,#4393,.T.);
#9030=EDGE_CURVE('',#6934,#6930,#507,.T.);
#9031=EDGE_CURVE('',#6931,#6935,#508,.T.);
#9032=EDGE_CURVE('',#6936,#6937,#4394,.T.);
#9033=EDGE_CURVE('',#6936,#6934,#509,.T.);
#9034=EDGE_CURVE('',#6935,#6937,#510,.T.);
#9035=EDGE_CURVE('',#6938,#6939,#4395,.T.);
#9036=EDGE_CURVE('',#6938,#6936,#511,.T.);
#9037=EDGE_CURVE('',#6937,#6939,#512,.T.);
#9038=EDGE_CURVE('',#6940,#6941,#4396,.T.);
#9039=EDGE_CURVE('',#6940,#6938,#513,.T.);
#9040=EDGE_CURVE('',#6939,#6941,#514,.T.);
#9041=EDGE_CURVE('',#6942,#6943,#4397,.T.);
#9042=EDGE_CURVE('',#6942,#6940,#515,.T.);
#9043=EDGE_CURVE('',#6941,#6943,#516,.T.);
#9044=EDGE_CURVE('',#6944,#6945,#4398,.T.);
#9045=EDGE_CURVE('',#6944,#6942,#517,.T.);
#9046=EDGE_CURVE('',#6943,#6945,#518,.T.);
#9047=EDGE_CURVE('',#6946,#6947,#4399,.T.);
#9048=EDGE_CURVE('',#6946,#6944,#519,.T.);
#9049=EDGE_CURVE('',#6945,#6947,#520,.T.);
#9050=EDGE_CURVE('',#6948,#6949,#4400,.T.);
#9051=EDGE_CURVE('',#6948,#6946,#521,.T.);
#9052=EDGE_CURVE('',#6947,#6949,#522,.T.);
#9053=EDGE_CURVE('',#6950,#6951,#4401,.T.);
#9054=EDGE_CURVE('',#6950,#6948,#523,.T.);
#9055=EDGE_CURVE('',#6949,#6951,#524,.T.);
#9056=EDGE_CURVE('',#6952,#6953,#4402,.T.);
#9057=EDGE_CURVE('',#6952,#6950,#525,.T.);
#9058=EDGE_CURVE('',#6951,#6953,#526,.T.);
#9059=EDGE_CURVE('',#6954,#6955,#4403,.T.);
#9060=EDGE_CURVE('',#6954,#6952,#527,.T.);
#9061=EDGE_CURVE('',#6953,#6955,#528,.T.);
#9062=EDGE_CURVE('',#6956,#6957,#4404,.T.);
#9063=EDGE_CURVE('',#6956,#6954,#529,.T.);
#9064=EDGE_CURVE('',#6955,#6957,#530,.T.);
#9065=EDGE_CURVE('',#6958,#6959,#4405,.T.);
#9066=EDGE_CURVE('',#6958,#6956,#531,.T.);
#9067=EDGE_CURVE('',#6957,#6959,#532,.T.);
#9068=EDGE_CURVE('',#6960,#6961,#4406,.T.);
#9069=EDGE_CURVE('',#6960,#6958,#533,.T.);
#9070=EDGE_CURVE('',#6959,#6961,#534,.T.);
#9071=EDGE_CURVE('',#6962,#6963,#4407,.T.);
#9072=EDGE_CURVE('',#6962,#6960,#535,.T.);
#9073=EDGE_CURVE('',#6961,#6963,#536,.T.);
#9074=EDGE_CURVE('',#6964,#6965,#4408,.T.);
#9075=EDGE_CURVE('',#6964,#6962,#537,.T.);
#9076=EDGE_CURVE('',#6963,#6965,#538,.T.);
#9077=EDGE_CURVE('',#6966,#6967,#4409,.T.);
#9078=EDGE_CURVE('',#6968,#6966,#1272,.T.);
#9079=EDGE_CURVE('',#6968,#6964,#539,.T.);
#9080=EDGE_CURVE('',#6965,#6967,#540,.T.);
#9081=EDGE_CURVE('',#6969,#6970,#4410,.T.);
#9082=EDGE_CURVE('',#6969,#6971,#541,.T.);
#9083=EDGE_CURVE('',#6972,#6971,#1273,.T.);
#9084=EDGE_CURVE('',#6970,#6972,#542,.T.);
#9085=EDGE_CURVE('',#6973,#6974,#4411,.T.);
#9086=EDGE_CURVE('',#6973,#6969,#543,.T.);
#9087=EDGE_CURVE('',#6974,#6970,#544,.T.);
#9088=EDGE_CURVE('',#6975,#6976,#4412,.T.);
#9089=EDGE_CURVE('',#6975,#6973,#545,.T.);
#9090=EDGE_CURVE('',#6976,#6974,#546,.T.);
#9091=EDGE_CURVE('',#6977,#6978,#4413,.T.);
#9092=EDGE_CURVE('',#6977,#6975,#547,.T.);
#9093=EDGE_CURVE('',#6978,#6976,#548,.T.);
#9094=EDGE_CURVE('',#6979,#6980,#4414,.T.);
#9095=EDGE_CURVE('',#6979,#6977,#549,.T.);
#9096=EDGE_CURVE('',#6980,#6978,#550,.T.);
#9097=EDGE_CURVE('',#6981,#6982,#4415,.T.);
#9098=EDGE_CURVE('',#6981,#6979,#551,.T.);
#9099=EDGE_CURVE('',#6982,#6980,#552,.T.);
#9100=EDGE_CURVE('',#6983,#6984,#4416,.T.);
#9101=EDGE_CURVE('',#6983,#6981,#553,.T.);
#9102=EDGE_CURVE('',#6984,#6982,#554,.T.);
#9103=EDGE_CURVE('',#6985,#6986,#4417,.T.);
#9104=EDGE_CURVE('',#6985,#6983,#555,.T.);
#9105=EDGE_CURVE('',#6986,#6984,#556,.T.);
#9106=EDGE_CURVE('',#6987,#6988,#4418,.T.);
#9107=EDGE_CURVE('',#6987,#6985,#557,.T.);
#9108=EDGE_CURVE('',#6988,#6986,#558,.T.);
#9109=EDGE_CURVE('',#6989,#6990,#4419,.T.);
#9110=EDGE_CURVE('',#6989,#6987,#559,.T.);
#9111=EDGE_CURVE('',#6990,#6988,#560,.T.);
#9112=EDGE_CURVE('',#6991,#6992,#4420,.T.);
#9113=EDGE_CURVE('',#6991,#6989,#561,.T.);
#9114=EDGE_CURVE('',#6992,#6990,#562,.T.);
#9115=EDGE_CURVE('',#6993,#6994,#4421,.T.);
#9116=EDGE_CURVE('',#6993,#6991,#563,.T.);
#9117=EDGE_CURVE('',#6994,#6992,#564,.T.);
#9118=EDGE_CURVE('',#6995,#6996,#4422,.T.);
#9119=EDGE_CURVE('',#6995,#6993,#565,.T.);
#9120=EDGE_CURVE('',#6996,#6994,#566,.T.);
#9121=EDGE_CURVE('',#6997,#6998,#4423,.T.);
#9122=EDGE_CURVE('',#6997,#6995,#567,.T.);
#9123=EDGE_CURVE('',#6998,#6996,#568,.T.);
#9124=EDGE_CURVE('',#6999,#7000,#4424,.T.);
#9125=EDGE_CURVE('',#6999,#6997,#569,.T.);
#9126=EDGE_CURVE('',#7000,#6998,#570,.T.);
#9127=EDGE_CURVE('',#7001,#7002,#4425,.T.);
#9128=EDGE_CURVE('',#7001,#6999,#571,.T.);
#9129=EDGE_CURVE('',#7002,#7000,#572,.T.);
#9130=EDGE_CURVE('',#7003,#7004,#4426,.T.);
#9131=EDGE_CURVE('',#7003,#7001,#573,.T.);
#9132=EDGE_CURVE('',#7004,#7002,#574,.T.);
#9133=EDGE_CURVE('',#7005,#6972,#575,.T.);
#9134=EDGE_CURVE('',#6967,#7005,#576,.T.);
#9135=EDGE_CURVE('',#7006,#6933,#577,.T.);
#9136=EDGE_CURVE('',#7006,#7004,#578,.T.);
#9137=EDGE_CURVE('',#6933,#7007,#1274,.T.);
#9138=EDGE_CURVE('',#7007,#6932,#1275,.T.);
#9139=EDGE_CURVE('',#6932,#7008,#579,.T.);
#9140=EDGE_CURVE('',#7008,#7006,#1276,.T.);
#9141=EDGE_CURVE('',#7008,#7003,#580,.T.);
#9142=EDGE_CURVE('',#6971,#6968,#581,.T.);
#9143=EDGE_CURVE('',#7009,#7010,#4427,.T.);
#9144=EDGE_CURVE('',#7010,#7010,#1277,.T.);
#9145=EDGE_CURVE('',#7011,#7012,#582,.T.);
#9146=EDGE_CURVE('',#7011,#7013,#4428,.T.);
#9147=EDGE_CURVE('',#7013,#7014,#4429,.T.);
#9148=EDGE_CURVE('',#7012,#7014,#4430,.T.);
#9149=EDGE_CURVE('',#7012,#7015,#583,.T.);
#9150=EDGE_CURVE('',#7014,#7016,#4431,.T.);
#9151=EDGE_CURVE('',#7015,#7016,#4432,.T.);
#9152=EDGE_CURVE('',#7015,#7017,#584,.T.);
#9153=EDGE_CURVE('',#7016,#7018,#4433,.T.);
#9154=EDGE_CURVE('',#7017,#7018,#4434,.T.);
#9155=EDGE_CURVE('',#7017,#7019,#585,.T.);
#9156=EDGE_CURVE('',#7018,#7020,#4435,.T.);
#9157=EDGE_CURVE('',#7019,#7020,#4436,.T.);
#9158=EDGE_CURVE('',#7021,#7011,#586,.T.);
#9159=EDGE_CURVE('',#7021,#7022,#4437,.T.);
#9160=EDGE_CURVE('',#7022,#7013,#4438,.T.);
#9161=EDGE_CURVE('',#7019,#7021,#587,.T.);
#9162=EDGE_CURVE('',#7020,#7022,#4439,.T.);
#9163=EDGE_CURVE('',#7023,#7023,#1278,.T.);
#9164=EDGE_CURVE('',#7007,#7023,#4440,.T.);
#9165=EDGE_CURVE('',#6966,#7005,#1279,.T.);
#9166=EDGE_CURVE('',#7024,#7024,#1280,.T.);
#9167=EDGE_CURVE('',#7025,#7026,#1281,.T.);
#9168=EDGE_CURVE('',#7025,#7024,#4441,.T.);
#9169=EDGE_CURVE('',#7026,#7025,#1282,.T.);
#9170=EDGE_CURVE('',#7017,#7026,#3202,.T.);
#9171=ORIENTED_EDGE('',*,*,#7027,.T.);
#9172=ORIENTED_EDGE('',*,*,#7028,.T.);
#9173=ORIENTED_EDGE('',*,*,#7029,.T.);
#9174=ORIENTED_EDGE('',*,*,#7030,.T.);
#9175=ORIENTED_EDGE('',*,*,#7031,.T.);
#9176=ORIENTED_EDGE('',*,*,#7032,.T.);
#9177=ORIENTED_EDGE('',*,*,#7027,.F.);
#9178=ORIENTED_EDGE('',*,*,#7033,.T.);
#9179=ORIENTED_EDGE('',*,*,#7034,.T.);
#9180=ORIENTED_EDGE('',*,*,#7035,.T.);
#9181=ORIENTED_EDGE('',*,*,#7036,.T.);
#9182=ORIENTED_EDGE('',*,*,#7032,.F.);
#9183=ORIENTED_EDGE('',*,*,#7037,.T.);
#9184=ORIENTED_EDGE('',*,*,#7038,.F.);
#9185=ORIENTED_EDGE('',*,*,#7039,.F.);
#9186=ORIENTED_EDGE('',*,*,#7040,.T.);
#9187=ORIENTED_EDGE('',*,*,#7033,.F.);
#9188=ORIENTED_EDGE('',*,*,#7031,.F.);
#9189=ORIENTED_EDGE('',*,*,#7041,.F.);
#9190=ORIENTED_EDGE('',*,*,#7042,.F.);
#9191=ORIENTED_EDGE('',*,*,#7037,.F.);
#9192=ORIENTED_EDGE('',*,*,#7043,.F.);
#9193=ORIENTED_EDGE('',*,*,#7044,.F.);
#9194=ORIENTED_EDGE('',*,*,#7035,.F.);
#9195=ORIENTED_EDGE('',*,*,#7045,.F.);
#9196=ORIENTED_EDGE('',*,*,#7046,.F.);
#9197=ORIENTED_EDGE('',*,*,#7047,.F.);
#9198=ORIENTED_EDGE('',*,*,#7048,.T.);
#9199=ORIENTED_EDGE('',*,*,#7049,.T.);
#9200=ORIENTED_EDGE('',*,*,#7046,.T.);
#9201=ORIENTED_EDGE('',*,*,#7050,.T.);
#9202=ORIENTED_EDGE('',*,*,#7048,.F.);
#9203=ORIENTED_EDGE('',*,*,#7051,.T.);
#9204=ORIENTED_EDGE('',*,*,#7052,.T.);
#9205=ORIENTED_EDGE('',*,*,#7053,.T.);
#9206=ORIENTED_EDGE('',*,*,#7054,.T.);
#9207=ORIENTED_EDGE('',*,*,#7055,.T.);
#9208=ORIENTED_EDGE('',*,*,#7052,.F.);
#9209=ORIENTED_EDGE('',*,*,#7056,.T.);
#9210=ORIENTED_EDGE('',*,*,#7029,.F.);
#9211=ORIENTED_EDGE('',*,*,#7057,.T.);
#9212=ORIENTED_EDGE('',*,*,#7047,.T.);
#9213=ORIENTED_EDGE('',*,*,#7058,.T.);
#9214=ORIENTED_EDGE('',*,*,#7059,.T.);
#9215=ORIENTED_EDGE('',*,*,#7044,.T.);
#9216=ORIENTED_EDGE('',*,*,#7060,.T.);
#9217=ORIENTED_EDGE('',*,*,#7045,.T.);
#9218=ORIENTED_EDGE('',*,*,#7061,.T.);
#9219=ORIENTED_EDGE('',*,*,#7062,.T.);
#9220=ORIENTED_EDGE('',*,*,#7063,.T.);
#9221=ORIENTED_EDGE('',*,*,#7064,.T.);
#9222=ORIENTED_EDGE('',*,*,#7065,.T.);
#9223=ORIENTED_EDGE('',*,*,#7064,.F.);
#9224=ORIENTED_EDGE('',*,*,#7066,.T.);
#9225=ORIENTED_EDGE('',*,*,#7067,.T.);
#9226=ORIENTED_EDGE('',*,*,#7068,.T.);
#9227=ORIENTED_EDGE('',*,*,#7067,.F.);
#9228=ORIENTED_EDGE('',*,*,#7069,.T.);
#9229=ORIENTED_EDGE('',*,*,#7043,.T.);
#9230=ORIENTED_EDGE('',*,*,#7070,.T.);
#9231=ORIENTED_EDGE('',*,*,#7058,.F.);
#9232=ORIENTED_EDGE('',*,*,#7049,.F.);
#9233=ORIENTED_EDGE('',*,*,#7053,.F.);
#9234=ORIENTED_EDGE('',*,*,#7055,.F.);
#9235=ORIENTED_EDGE('',*,*,#7071,.F.);
#9236=ORIENTED_EDGE('',*,*,#7072,.F.);
#9237=ORIENTED_EDGE('',*,*,#7073,.F.);
#9238=ORIENTED_EDGE('',*,*,#7074,.F.);
#9239=ORIENTED_EDGE('',*,*,#7075,.F.);
#9240=ORIENTED_EDGE('',*,*,#7076,.F.);
#9241=ORIENTED_EDGE('',*,*,#7050,.F.);
#9242=ORIENTED_EDGE('',*,*,#7060,.F.);
#9243=ORIENTED_EDGE('',*,*,#7069,.F.);
#9244=ORIENTED_EDGE('',*,*,#7077,.F.);
#9245=ORIENTED_EDGE('',*,*,#7051,.F.);
#9246=ORIENTED_EDGE('',*,*,#7077,.T.);
#9247=ORIENTED_EDGE('',*,*,#7066,.F.);
#9248=ORIENTED_EDGE('',*,*,#7078,.T.);
#9249=ORIENTED_EDGE('',*,*,#7056,.F.);
#9250=ORIENTED_EDGE('',*,*,#7078,.F.);
#9251=ORIENTED_EDGE('',*,*,#7063,.F.);
#9252=ORIENTED_EDGE('',*,*,#7079,.F.);
#9253=ORIENTED_EDGE('',*,*,#7080,.F.);
#9254=ORIENTED_EDGE('',*,*,#7081,.F.);
#9255=ORIENTED_EDGE('',*,*,#7082,.T.);
#9256=ORIENTED_EDGE('',*,*,#7083,.T.);
#9257=ORIENTED_EDGE('',*,*,#7084,.T.);
#9258=ORIENTED_EDGE('',*,*,#7085,.T.);
#9259=ORIENTED_EDGE('',*,*,#7038,.T.);
#9260=ORIENTED_EDGE('',*,*,#7042,.T.);
#9261=ORIENTED_EDGE('',*,*,#7086,.T.);
#9262=ORIENTED_EDGE('',*,*,#7085,.F.);
#9263=ORIENTED_EDGE('',*,*,#7087,.T.);
#9264=ORIENTED_EDGE('',*,*,#7088,.T.);
#9265=ORIENTED_EDGE('',*,*,#7089,.T.);
#9266=ORIENTED_EDGE('',*,*,#7039,.T.);
#9267=ORIENTED_EDGE('',*,*,#7088,.F.);
#9268=ORIENTED_EDGE('',*,*,#7090,.F.);
#9269=ORIENTED_EDGE('',*,*,#7091,.F.);
#9270=ORIENTED_EDGE('',*,*,#7092,.F.);
#9271=ORIENTED_EDGE('',*,*,#7093,.F.);
#9272=ORIENTED_EDGE('',*,*,#7094,.F.);
#9273=ORIENTED_EDGE('',*,*,#7083,.F.);
#9274=ORIENTED_EDGE('',*,*,#7095,.T.);
#9275=ORIENTED_EDGE('',*,*,#7075,.T.);
#9276=ORIENTED_EDGE('',*,*,#7093,.T.);
#9277=ORIENTED_EDGE('',*,*,#7096,.T.);
#9278=ORIENTED_EDGE('',*,*,#7097,.T.);
#9279=ORIENTED_EDGE('',*,*,#7098,.T.);
#9280=ORIENTED_EDGE('',*,*,#7099,.T.);
#9281=ORIENTED_EDGE('',*,*,#7072,.T.);
#9282=ORIENTED_EDGE('',*,*,#7099,.F.);
#9283=ORIENTED_EDGE('',*,*,#7100,.T.);
#9284=ORIENTED_EDGE('',*,*,#7101,.T.);
#9285=ORIENTED_EDGE('',*,*,#7073,.T.);
#9286=ORIENTED_EDGE('',*,*,#7101,.F.);
#9287=ORIENTED_EDGE('',*,*,#7102,.T.);
#9288=ORIENTED_EDGE('',*,*,#7094,.T.);
#9289=ORIENTED_EDGE('',*,*,#7074,.T.);
#9290=ORIENTED_EDGE('',*,*,#7090,.T.);
#9291=ORIENTED_EDGE('',*,*,#7103,.T.);
#9292=ORIENTED_EDGE('',*,*,#7092,.T.);
#9293=ORIENTED_EDGE('',*,*,#7104,.T.);
#9294=ORIENTED_EDGE('',*,*,#7105,.T.);
#9295=ORIENTED_EDGE('',*,*,#7106,.T.);
#9296=ORIENTED_EDGE('',*,*,#7091,.T.);
#9297=ORIENTED_EDGE('',*,*,#7107,.T.);
#9298=ORIENTED_EDGE('',*,*,#7105,.F.);
#9299=ORIENTED_EDGE('',*,*,#7108,.T.);
#9300=ORIENTED_EDGE('',*,*,#7109,.T.);
#9301=ORIENTED_EDGE('',*,*,#7110,.T.);
#9302=ORIENTED_EDGE('',*,*,#7111,.T.);
#9303=ORIENTED_EDGE('',*,*,#7112,.T.);
#9304=ORIENTED_EDGE('',*,*,#7109,.F.);
#9305=ORIENTED_EDGE('',*,*,#7113,.T.);
#9306=ORIENTED_EDGE('',*,*,#7030,.F.);
#9307=ORIENTED_EDGE('',*,*,#7059,.F.);
#9308=ORIENTED_EDGE('',*,*,#7076,.T.);
#9309=ORIENTED_EDGE('',*,*,#7095,.F.);
#9310=ORIENTED_EDGE('',*,*,#7086,.F.);
#9311=ORIENTED_EDGE('',*,*,#7041,.T.);
#9312=ORIENTED_EDGE('',*,*,#7084,.F.);
#9313=ORIENTED_EDGE('',*,*,#7096,.F.);
#9314=ORIENTED_EDGE('',*,*,#7103,.F.);
#9315=ORIENTED_EDGE('',*,*,#7087,.F.);
#9316=ORIENTED_EDGE('',*,*,#7114,.T.);
#9317=ORIENTED_EDGE('',*,*,#7115,.T.);
#9318=ORIENTED_EDGE('',*,*,#7097,.F.);
#9319=ORIENTED_EDGE('',*,*,#7071,.T.);
#9320=ORIENTED_EDGE('',*,*,#7054,.F.);
#9321=ORIENTED_EDGE('',*,*,#7081,.T.);
#9322=ORIENTED_EDGE('',*,*,#7116,.T.);
#9323=ORIENTED_EDGE('',*,*,#7117,.T.);
#9324=ORIENTED_EDGE('',*,*,#7118,.T.);
#9325=ORIENTED_EDGE('',*,*,#7079,.T.);
#9326=ORIENTED_EDGE('',*,*,#7062,.F.);
#9327=ORIENTED_EDGE('',*,*,#7119,.T.);
#9328=ORIENTED_EDGE('',*,*,#7111,.F.);
#9329=ORIENTED_EDGE('',*,*,#7116,.F.);
#9330=ORIENTED_EDGE('',*,*,#7080,.T.);
#9331=ORIENTED_EDGE('',*,*,#7118,.F.);
#9332=ORIENTED_EDGE('',*,*,#7120,.F.);
#9333=ORIENTED_EDGE('',*,*,#7082,.F.);
#9334=ORIENTED_EDGE('',*,*,#7121,.T.);
#9335=ORIENTED_EDGE('',*,*,#7122,.F.);
#9336=ORIENTED_EDGE('',*,*,#7121,.F.);
#9337=ORIENTED_EDGE('',*,*,#7123,.F.);
#9338=ORIENTED_EDGE('',*,*,#7124,.T.);
#9339=ORIENTED_EDGE('',*,*,#7114,.F.);
#9340=ORIENTED_EDGE('',*,*,#7124,.F.);
#9341=ORIENTED_EDGE('',*,*,#7034,.F.);
#9342=ORIENTED_EDGE('',*,*,#7040,.F.);
#9343=ORIENTED_EDGE('',*,*,#7089,.F.);
#9344=ORIENTED_EDGE('',*,*,#7106,.F.);
#9345=ORIENTED_EDGE('',*,*,#7110,.F.);
#9346=ORIENTED_EDGE('',*,*,#7112,.F.);
#9347=ORIENTED_EDGE('',*,*,#7119,.F.);
#9348=ORIENTED_EDGE('',*,*,#7065,.F.);
#9349=ORIENTED_EDGE('',*,*,#7068,.F.);
#9350=ORIENTED_EDGE('',*,*,#7070,.F.);
#9351=ORIENTED_EDGE('',*,*,#7100,.F.);
#9352=ORIENTED_EDGE('',*,*,#7125,.T.);
#9353=ORIENTED_EDGE('',*,*,#7108,.F.);
#9354=ORIENTED_EDGE('',*,*,#7126,.T.);
#9355=ORIENTED_EDGE('',*,*,#7098,.F.);
#9356=ORIENTED_EDGE('',*,*,#7115,.F.);
#9357=ORIENTED_EDGE('',*,*,#7120,.T.);
#9358=ORIENTED_EDGE('',*,*,#7117,.F.);
#9359=ORIENTED_EDGE('',*,*,#7113,.F.);
#9360=ORIENTED_EDGE('',*,*,#7125,.F.);
#9361=ORIENTED_EDGE('',*,*,#7123,.T.);
#9362=ORIENTED_EDGE('',*,*,#7102,.F.);
#9363=ORIENTED_EDGE('',*,*,#7126,.F.);
#9364=ORIENTED_EDGE('',*,*,#7107,.F.);
#9365=ORIENTED_EDGE('',*,*,#7104,.F.);
#9366=ORIENTED_EDGE('',*,*,#7028,.F.);
#9367=ORIENTED_EDGE('',*,*,#7036,.F.);
#9368=ORIENTED_EDGE('',*,*,#7061,.F.);
#9369=ORIENTED_EDGE('',*,*,#7057,.F.);
#9370=ORIENTED_EDGE('',*,*,#7122,.T.);
#9371=ORIENTED_EDGE('',*,*,#7127,.T.);
#9372=ORIENTED_EDGE('',*,*,#7128,.T.);
#9373=ORIENTED_EDGE('',*,*,#7129,.T.);
#9374=ORIENTED_EDGE('',*,*,#7130,.T.);
#9375=ORIENTED_EDGE('',*,*,#7129,.F.);
#9376=ORIENTED_EDGE('',*,*,#7131,.T.);
#9377=ORIENTED_EDGE('',*,*,#7132,.T.);
#9378=ORIENTED_EDGE('',*,*,#7133,.T.);
#9379=ORIENTED_EDGE('',*,*,#7134,.T.);
#9380=ORIENTED_EDGE('',*,*,#7135,.T.);
#9381=ORIENTED_EDGE('',*,*,#7132,.F.);
#9382=ORIENTED_EDGE('',*,*,#7136,.T.);
#9383=ORIENTED_EDGE('',*,*,#7134,.F.);
#9384=ORIENTED_EDGE('',*,*,#7137,.T.);
#9385=ORIENTED_EDGE('',*,*,#7138,.T.);
#9386=ORIENTED_EDGE('',*,*,#7139,.T.);
#9387=ORIENTED_EDGE('',*,*,#7140,.T.);
#9388=ORIENTED_EDGE('',*,*,#7138,.F.);
#9389=ORIENTED_EDGE('',*,*,#7141,.T.);
#9390=ORIENTED_EDGE('',*,*,#7142,.T.);
#9391=ORIENTED_EDGE('',*,*,#7143,.T.);
#9392=ORIENTED_EDGE('',*,*,#7144,.T.);
#9393=ORIENTED_EDGE('',*,*,#7145,.T.);
#9394=ORIENTED_EDGE('',*,*,#7142,.F.);
#9395=ORIENTED_EDGE('',*,*,#7130,.F.);
#9396=ORIENTED_EDGE('',*,*,#7133,.F.);
#9397=ORIENTED_EDGE('',*,*,#7135,.F.);
#9398=ORIENTED_EDGE('',*,*,#7139,.F.);
#9399=ORIENTED_EDGE('',*,*,#7140,.F.);
#9400=ORIENTED_EDGE('',*,*,#7146,.F.);
#9401=ORIENTED_EDGE('',*,*,#7147,.T.);
#9402=ORIENTED_EDGE('',*,*,#7145,.F.);
#9403=ORIENTED_EDGE('',*,*,#7148,.F.);
#9404=ORIENTED_EDGE('',*,*,#7149,.F.);
#9405=ORIENTED_EDGE('',*,*,#7150,.F.);
#9406=ORIENTED_EDGE('',*,*,#7151,.F.);
#9407=ORIENTED_EDGE('',*,*,#7146,.T.);
#9408=ORIENTED_EDGE('',*,*,#7152,.T.);
#9409=ORIENTED_EDGE('',*,*,#7153,.T.);
#9410=ORIENTED_EDGE('',*,*,#7154,.T.);
#9411=ORIENTED_EDGE('',*,*,#7155,.T.);
#9412=ORIENTED_EDGE('',*,*,#7156,.T.);
#9413=ORIENTED_EDGE('',*,*,#7157,.T.);
#9414=ORIENTED_EDGE('',*,*,#7158,.T.);
#9415=ORIENTED_EDGE('',*,*,#7159,.T.);
#9416=ORIENTED_EDGE('',*,*,#7160,.T.);
#9417=ORIENTED_EDGE('',*,*,#7161,.T.);
#9418=ORIENTED_EDGE('',*,*,#7162,.T.);
#9419=ORIENTED_EDGE('',*,*,#7159,.F.);
#9420=ORIENTED_EDGE('',*,*,#7163,.T.);
#9421=ORIENTED_EDGE('',*,*,#7164,.T.);
#9422=ORIENTED_EDGE('',*,*,#7161,.F.);
#9423=ORIENTED_EDGE('',*,*,#7165,.T.);
#9424=ORIENTED_EDGE('',*,*,#7166,.T.);
#9425=ORIENTED_EDGE('',*,*,#7167,.T.);
#9426=ORIENTED_EDGE('',*,*,#7163,.F.);
#9427=ORIENTED_EDGE('',*,*,#7168,.T.);
#9428=ORIENTED_EDGE('',*,*,#7169,.T.);
#9429=ORIENTED_EDGE('',*,*,#7170,.T.);
#9430=ORIENTED_EDGE('',*,*,#7171,.T.);
#9431=ORIENTED_EDGE('',*,*,#7157,.F.);
#9432=ORIENTED_EDGE('',*,*,#7172,.T.);
#9433=ORIENTED_EDGE('',*,*,#7173,.T.);
#9434=ORIENTED_EDGE('',*,*,#7174,.T.);
#9435=ORIENTED_EDGE('',*,*,#7170,.F.);
#9436=ORIENTED_EDGE('',*,*,#7175,.T.);
#9437=ORIENTED_EDGE('',*,*,#7176,.T.);
#9438=ORIENTED_EDGE('',*,*,#7177,.T.);
#9439=ORIENTED_EDGE('',*,*,#7173,.F.);
#9440=ORIENTED_EDGE('',*,*,#7178,.T.);
#9441=ORIENTED_EDGE('',*,*,#7179,.T.);
#9442=ORIENTED_EDGE('',*,*,#7176,.F.);
#9443=ORIENTED_EDGE('',*,*,#7180,.T.);
#9444=ORIENTED_EDGE('',*,*,#7155,.F.);
#9445=ORIENTED_EDGE('',*,*,#7153,.F.);
#9446=ORIENTED_EDGE('',*,*,#7181,.T.);
#9447=ORIENTED_EDGE('',*,*,#7182,.T.);
#9448=ORIENTED_EDGE('',*,*,#7183,.T.);
#9449=ORIENTED_EDGE('',*,*,#7184,.T.);
#9450=ORIENTED_EDGE('',*,*,#7185,.T.);
#9451=ORIENTED_EDGE('',*,*,#7182,.F.);
#9452=ORIENTED_EDGE('',*,*,#7186,.T.);
#9453=ORIENTED_EDGE('',*,*,#7187,.T.);
#9454=ORIENTED_EDGE('',*,*,#7188,.F.);
#9455=ORIENTED_EDGE('',*,*,#7189,.F.);
#9456=ORIENTED_EDGE('',*,*,#7190,.F.);
#9457=ORIENTED_EDGE('',*,*,#7191,.F.);
#9458=ORIENTED_EDGE('',*,*,#7192,.F.);
#9459=ORIENTED_EDGE('',*,*,#7193,.F.);
#9460=ORIENTED_EDGE('',*,*,#7194,.F.);
#9461=ORIENTED_EDGE('',*,*,#7195,.F.);
#9462=ORIENTED_EDGE('',*,*,#7196,.F.);
#9463=ORIENTED_EDGE('',*,*,#7197,.F.);
#9464=ORIENTED_EDGE('',*,*,#7198,.F.);
#9465=ORIENTED_EDGE('',*,*,#7199,.F.);
#9466=ORIENTED_EDGE('',*,*,#7168,.F.);
#9467=ORIENTED_EDGE('',*,*,#7165,.F.);
#9468=ORIENTED_EDGE('',*,*,#7160,.F.);
#9469=ORIENTED_EDGE('',*,*,#7158,.F.);
#9470=ORIENTED_EDGE('',*,*,#7200,.F.);
#9471=ORIENTED_EDGE('',*,*,#7128,.F.);
#9472=ORIENTED_EDGE('',*,*,#7131,.F.);
#9473=ORIENTED_EDGE('',*,*,#7200,.T.);
#9474=ORIENTED_EDGE('',*,*,#7171,.F.);
#9475=ORIENTED_EDGE('',*,*,#7201,.T.);
#9476=ORIENTED_EDGE('',*,*,#7136,.F.);
#9477=ORIENTED_EDGE('',*,*,#7201,.F.);
#9478=ORIENTED_EDGE('',*,*,#7174,.F.);
#9479=ORIENTED_EDGE('',*,*,#7202,.F.);
#9480=ORIENTED_EDGE('',*,*,#7137,.F.);
#9481=ORIENTED_EDGE('',*,*,#7202,.T.);
#9482=ORIENTED_EDGE('',*,*,#7177,.F.);
#9483=ORIENTED_EDGE('',*,*,#7203,.T.);
#9484=ORIENTED_EDGE('',*,*,#7141,.F.);
#9485=ORIENTED_EDGE('',*,*,#7203,.F.);
#9486=ORIENTED_EDGE('',*,*,#7179,.F.);
#9487=ORIENTED_EDGE('',*,*,#7154,.F.);
#9488=ORIENTED_EDGE('',*,*,#7183,.F.);
#9489=ORIENTED_EDGE('',*,*,#7185,.F.);
#9490=ORIENTED_EDGE('',*,*,#7204,.F.);
#9491=ORIENTED_EDGE('',*,*,#7205,.F.);
#9492=ORIENTED_EDGE('',*,*,#7206,.F.);
#9493=ORIENTED_EDGE('',*,*,#7207,.F.);
#9494=ORIENTED_EDGE('',*,*,#7208,.F.);
#9495=ORIENTED_EDGE('',*,*,#7209,.F.);
#9496=ORIENTED_EDGE('',*,*,#7210,.F.);
#9497=ORIENTED_EDGE('',*,*,#7211,.F.);
#9498=ORIENTED_EDGE('',*,*,#7212,.F.);
#9499=ORIENTED_EDGE('',*,*,#7213,.F.);
#9500=ORIENTED_EDGE('',*,*,#7214,.F.);
#9501=ORIENTED_EDGE('',*,*,#7143,.F.);
#9502=ORIENTED_EDGE('',*,*,#7184,.F.);
#9503=ORIENTED_EDGE('',*,*,#7215,.F.);
#9504=ORIENTED_EDGE('',*,*,#7216,.T.);
#9505=ORIENTED_EDGE('',*,*,#7217,.T.);
#9506=ORIENTED_EDGE('',*,*,#7218,.T.);
#9507=ORIENTED_EDGE('',*,*,#7204,.T.);
#9508=ORIENTED_EDGE('',*,*,#7219,.T.);
#9509=ORIENTED_EDGE('',*,*,#7220,.T.);
#9510=ORIENTED_EDGE('',*,*,#7221,.T.);
#9511=ORIENTED_EDGE('',*,*,#7213,.T.);
#9512=ORIENTED_EDGE('',*,*,#7220,.F.);
#9513=ORIENTED_EDGE('',*,*,#7222,.F.);
#9514=ORIENTED_EDGE('',*,*,#7223,.F.);
#9515=ORIENTED_EDGE('',*,*,#7224,.F.);
#9516=ORIENTED_EDGE('',*,*,#7225,.T.);
#9517=ORIENTED_EDGE('',*,*,#7226,.F.);
#9518=ORIENTED_EDGE('',*,*,#7227,.F.);
#9519=ORIENTED_EDGE('',*,*,#7228,.F.);
#9520=ORIENTED_EDGE('',*,*,#7229,.F.);
#9521=ORIENTED_EDGE('',*,*,#7230,.T.);
#9522=ORIENTED_EDGE('',*,*,#7231,.T.);
#9523=ORIENTED_EDGE('',*,*,#7228,.T.);
#9524=ORIENTED_EDGE('',*,*,#7232,.T.);
#9525=ORIENTED_EDGE('',*,*,#7233,.T.);
#9526=ORIENTED_EDGE('',*,*,#7234,.T.);
#9527=ORIENTED_EDGE('',*,*,#7207,.T.);
#9528=ORIENTED_EDGE('',*,*,#7229,.T.);
#9529=ORIENTED_EDGE('',*,*,#7235,.T.);
#9530=ORIENTED_EDGE('',*,*,#7234,.F.);
#9531=ORIENTED_EDGE('',*,*,#7236,.T.);
#9532=ORIENTED_EDGE('',*,*,#7237,.T.);
#9533=ORIENTED_EDGE('',*,*,#7208,.T.);
#9534=ORIENTED_EDGE('',*,*,#7238,.T.);
#9535=ORIENTED_EDGE('',*,*,#7209,.T.);
#9536=ORIENTED_EDGE('',*,*,#7237,.F.);
#9537=ORIENTED_EDGE('',*,*,#7239,.T.);
#9538=ORIENTED_EDGE('',*,*,#7240,.T.);
#9539=ORIENTED_EDGE('',*,*,#7241,.T.);
#9540=ORIENTED_EDGE('',*,*,#7227,.T.);
#9541=ORIENTED_EDGE('',*,*,#7206,.T.);
#9542=ORIENTED_EDGE('',*,*,#7242,.T.);
#9543=ORIENTED_EDGE('',*,*,#7236,.F.);
#9544=ORIENTED_EDGE('',*,*,#7243,.T.);
#9545=ORIENTED_EDGE('',*,*,#7244,.F.);
#9546=ORIENTED_EDGE('',*,*,#7245,.T.);
#9547=ORIENTED_EDGE('',*,*,#7235,.F.);
#9548=ORIENTED_EDGE('',*,*,#7231,.F.);
#9549=ORIENTED_EDGE('',*,*,#7246,.F.);
#9550=ORIENTED_EDGE('',*,*,#7243,.F.);
#9551=ORIENTED_EDGE('',*,*,#7230,.F.);
#9552=ORIENTED_EDGE('',*,*,#7247,.F.);
#9553=ORIENTED_EDGE('',*,*,#7196,.T.);
#9554=ORIENTED_EDGE('',*,*,#7248,.T.);
#9555=ORIENTED_EDGE('',*,*,#7246,.T.);
#9556=ORIENTED_EDGE('',*,*,#7233,.F.);
#9557=ORIENTED_EDGE('',*,*,#7249,.T.);
#9558=ORIENTED_EDGE('',*,*,#7250,.T.);
#9559=ORIENTED_EDGE('',*,*,#7251,.T.);
#9560=ORIENTED_EDGE('',*,*,#7197,.T.);
#9561=ORIENTED_EDGE('',*,*,#7247,.T.);
#9562=ORIENTED_EDGE('',*,*,#7232,.F.);
#9563=ORIENTED_EDGE('',*,*,#7241,.F.);
#9564=ORIENTED_EDGE('',*,*,#7252,.F.);
#9565=ORIENTED_EDGE('',*,*,#7249,.F.);
#9566=ORIENTED_EDGE('',*,*,#7253,.T.);
#9567=ORIENTED_EDGE('',*,*,#7240,.F.);
#9568=ORIENTED_EDGE('',*,*,#7254,.T.);
#9569=ORIENTED_EDGE('',*,*,#7255,.T.);
#9570=ORIENTED_EDGE('',*,*,#7256,.T.);
#9571=ORIENTED_EDGE('',*,*,#7250,.F.);
#9572=ORIENTED_EDGE('',*,*,#7252,.T.);
#9573=ORIENTED_EDGE('',*,*,#7257,.T.);
#9574=ORIENTED_EDGE('',*,*,#7244,.T.);
#9575=ORIENTED_EDGE('',*,*,#7248,.F.);
#9576=ORIENTED_EDGE('',*,*,#7195,.T.);
#9577=ORIENTED_EDGE('',*,*,#7258,.T.);
#9578=ORIENTED_EDGE('',*,*,#7257,.F.);
#9579=ORIENTED_EDGE('',*,*,#7194,.T.);
#9580=ORIENTED_EDGE('',*,*,#7259,.T.);
#9581=ORIENTED_EDGE('',*,*,#7260,.T.);
#9582=ORIENTED_EDGE('',*,*,#7261,.T.);
#9583=ORIENTED_EDGE('',*,*,#7210,.T.);
#9584=ORIENTED_EDGE('',*,*,#7238,.F.);
#9585=ORIENTED_EDGE('',*,*,#7262,.T.);
#9586=ORIENTED_EDGE('',*,*,#7263,.T.);
#9587=ORIENTED_EDGE('',*,*,#7261,.F.);
#9588=ORIENTED_EDGE('',*,*,#7264,.T.);
#9589=ORIENTED_EDGE('',*,*,#7262,.F.);
#9590=ORIENTED_EDGE('',*,*,#7265,.T.);
#9591=ORIENTED_EDGE('',*,*,#7266,.T.);
#9592=ORIENTED_EDGE('',*,*,#7267,.T.);
#9593=ORIENTED_EDGE('',*,*,#7268,.T.);
#9594=ORIENTED_EDGE('',*,*,#7269,.T.);
#9595=ORIENTED_EDGE('',*,*,#7266,.F.);
#9596=ORIENTED_EDGE('',*,*,#7270,.T.);
#9597=ORIENTED_EDGE('',*,*,#7193,.T.);
#9598=ORIENTED_EDGE('',*,*,#7268,.F.);
#9599=ORIENTED_EDGE('',*,*,#7271,.T.);
#9600=ORIENTED_EDGE('',*,*,#7259,.F.);
#9601=ORIENTED_EDGE('',*,*,#7239,.F.);
#9602=ORIENTED_EDGE('',*,*,#7245,.F.);
#9603=ORIENTED_EDGE('',*,*,#7258,.F.);
#9604=ORIENTED_EDGE('',*,*,#7272,.T.);
#9605=ORIENTED_EDGE('',*,*,#7273,.T.);
#9606=ORIENTED_EDGE('',*,*,#7271,.F.);
#9607=ORIENTED_EDGE('',*,*,#7270,.F.);
#9608=ORIENTED_EDGE('',*,*,#7265,.F.);
#9609=ORIENTED_EDGE('',*,*,#7264,.F.);
#9610=ORIENTED_EDGE('',*,*,#7260,.F.);
#9611=ORIENTED_EDGE('',*,*,#7272,.F.);
#9612=ORIENTED_EDGE('',*,*,#7274,.T.);
#9613=ORIENTED_EDGE('',*,*,#7275,.T.);
#9614=ORIENTED_EDGE('',*,*,#7276,.T.);
#9615=ORIENTED_EDGE('',*,*,#7191,.T.);
#9616=ORIENTED_EDGE('',*,*,#7277,.T.);
#9617=ORIENTED_EDGE('',*,*,#7190,.T.);
#9618=ORIENTED_EDGE('',*,*,#7278,.T.);
#9619=ORIENTED_EDGE('',*,*,#7223,.T.);
#9620=ORIENTED_EDGE('',*,*,#7277,.F.);
#9621=ORIENTED_EDGE('',*,*,#7279,.T.);
#9622=ORIENTED_EDGE('',*,*,#7280,.T.);
#9623=ORIENTED_EDGE('',*,*,#7276,.F.);
#9624=ORIENTED_EDGE('',*,*,#7281,.T.);
#9625=ORIENTED_EDGE('',*,*,#7282,.T.);
#9626=ORIENTED_EDGE('',*,*,#7283,.T.);
#9627=ORIENTED_EDGE('',*,*,#7279,.F.);
#9628=ORIENTED_EDGE('',*,*,#7284,.T.);
#9629=ORIENTED_EDGE('',*,*,#7285,.T.);
#9630=ORIENTED_EDGE('',*,*,#7286,.T.);
#9631=ORIENTED_EDGE('',*,*,#7282,.F.);
#9632=ORIENTED_EDGE('',*,*,#7287,.T.);
#9633=ORIENTED_EDGE('',*,*,#7212,.T.);
#9634=ORIENTED_EDGE('',*,*,#7285,.F.);
#9635=ORIENTED_EDGE('',*,*,#7288,.T.);
#9636=ORIENTED_EDGE('',*,*,#7219,.F.);
#9637=ORIENTED_EDGE('',*,*,#7288,.F.);
#9638=ORIENTED_EDGE('',*,*,#7287,.F.);
#9639=ORIENTED_EDGE('',*,*,#7284,.F.);
#9640=ORIENTED_EDGE('',*,*,#7281,.F.);
#9641=ORIENTED_EDGE('',*,*,#7275,.F.);
#9642=ORIENTED_EDGE('',*,*,#7222,.T.);
#9643=ORIENTED_EDGE('',*,*,#7289,.T.);
#9644=ORIENTED_EDGE('',*,*,#7290,.T.);
#9645=ORIENTED_EDGE('',*,*,#7188,.T.);
#9646=ORIENTED_EDGE('',*,*,#7127,.F.);
#9647=ORIENTED_EDGE('',*,*,#7151,.T.);
#9648=ORIENTED_EDGE('',*,*,#7169,.F.);
#9649=ORIENTED_EDGE('',*,*,#7199,.T.);
#9650=ORIENTED_EDGE('',*,*,#7291,.T.);
#9651=ORIENTED_EDGE('',*,*,#7292,.T.);
#9652=ORIENTED_EDGE('',*,*,#7293,.T.);
#9653=ORIENTED_EDGE('',*,*,#7294,.T.);
#9654=ORIENTED_EDGE('',*,*,#7166,.F.);
#9655=ORIENTED_EDGE('',*,*,#7294,.F.);
#9656=ORIENTED_EDGE('',*,*,#7295,.T.);
#9657=ORIENTED_EDGE('',*,*,#7215,.T.);
#9658=ORIENTED_EDGE('',*,*,#7187,.F.);
#9659=ORIENTED_EDGE('',*,*,#7296,.T.);
#9660=ORIENTED_EDGE('',*,*,#7251,.F.);
#9661=ORIENTED_EDGE('',*,*,#7256,.F.);
#9662=ORIENTED_EDGE('',*,*,#7297,.T.);
#9663=ORIENTED_EDGE('',*,*,#7298,.F.);
#9664=ORIENTED_EDGE('',*,*,#7291,.F.);
#9665=ORIENTED_EDGE('',*,*,#7198,.T.);
#9666=ORIENTED_EDGE('',*,*,#7167,.F.);
#9667=ORIENTED_EDGE('',*,*,#7296,.F.);
#9668=ORIENTED_EDGE('',*,*,#7186,.F.);
#9669=ORIENTED_EDGE('',*,*,#7299,.F.);
#9670=ORIENTED_EDGE('',*,*,#7242,.F.);
#9671=ORIENTED_EDGE('',*,*,#7205,.T.);
#9672=ORIENTED_EDGE('',*,*,#7218,.F.);
#9673=ORIENTED_EDGE('',*,*,#7300,.F.);
#9674=ORIENTED_EDGE('',*,*,#7301,.T.);
#9675=ORIENTED_EDGE('',*,*,#7254,.F.);
#9676=ORIENTED_EDGE('',*,*,#7255,.F.);
#9677=ORIENTED_EDGE('',*,*,#7301,.F.);
#9678=ORIENTED_EDGE('',*,*,#7302,.F.);
#9679=ORIENTED_EDGE('',*,*,#7297,.F.);
#9680=ORIENTED_EDGE('',*,*,#7303,.F.);
#9681=ORIENTED_EDGE('',*,*,#7304,.F.);
#9682=ORIENTED_EDGE('',*,*,#7305,.F.);
#9683=ORIENTED_EDGE('',*,*,#7306,.F.);
#9684=ORIENTED_EDGE('',*,*,#7292,.F.);
#9685=ORIENTED_EDGE('',*,*,#7298,.T.);
#9686=ORIENTED_EDGE('',*,*,#7302,.T.);
#9687=ORIENTED_EDGE('',*,*,#7300,.T.);
#9688=ORIENTED_EDGE('',*,*,#7217,.F.);
#9689=ORIENTED_EDGE('',*,*,#7307,.T.);
#9690=ORIENTED_EDGE('',*,*,#7305,.T.);
#9691=ORIENTED_EDGE('',*,*,#7308,.T.);
#9692=ORIENTED_EDGE('',*,*,#7309,.T.);
#9693=ORIENTED_EDGE('',*,*,#7310,.T.);
#9694=ORIENTED_EDGE('',*,*,#7303,.T.);
#9695=ORIENTED_EDGE('',*,*,#7311,.T.);
#9696=ORIENTED_EDGE('',*,*,#7312,.T.);
#9697=ORIENTED_EDGE('',*,*,#7313,.T.);
#9698=ORIENTED_EDGE('',*,*,#7314,.T.);
#9699=ORIENTED_EDGE('',*,*,#7315,.T.);
#9700=ORIENTED_EDGE('',*,*,#7311,.F.);
#9701=ORIENTED_EDGE('',*,*,#7306,.T.);
#9702=ORIENTED_EDGE('',*,*,#7310,.F.);
#9703=ORIENTED_EDGE('',*,*,#7316,.T.);
#9704=ORIENTED_EDGE('',*,*,#7304,.T.);
#9705=ORIENTED_EDGE('',*,*,#7313,.F.);
#9706=ORIENTED_EDGE('',*,*,#7317,.T.);
#9707=ORIENTED_EDGE('',*,*,#7318,.T.);
#9708=ORIENTED_EDGE('',*,*,#7319,.T.);
#9709=ORIENTED_EDGE('',*,*,#7308,.F.);
#9710=ORIENTED_EDGE('',*,*,#7318,.F.);
#9711=ORIENTED_EDGE('',*,*,#7320,.F.);
#9712=ORIENTED_EDGE('',*,*,#7321,.F.);
#9713=ORIENTED_EDGE('',*,*,#7322,.F.);
#9714=ORIENTED_EDGE('',*,*,#7323,.F.);
#9715=ORIENTED_EDGE('',*,*,#7324,.F.);
#9716=ORIENTED_EDGE('',*,*,#7312,.F.);
#9717=ORIENTED_EDGE('',*,*,#7315,.F.);
#9718=ORIENTED_EDGE('',*,*,#7325,.T.);
#9719=ORIENTED_EDGE('',*,*,#7326,.F.);
#9720=ORIENTED_EDGE('',*,*,#7320,.T.);
#9721=ORIENTED_EDGE('',*,*,#7317,.F.);
#9722=ORIENTED_EDGE('',*,*,#7327,.T.);
#9723=ORIENTED_EDGE('',*,*,#7328,.T.);
#9724=ORIENTED_EDGE('',*,*,#7329,.T.);
#9725=ORIENTED_EDGE('',*,*,#7330,.T.);
#9726=ORIENTED_EDGE('',*,*,#7331,.T.);
#9727=ORIENTED_EDGE('',*,*,#7332,.T.);
#9728=ORIENTED_EDGE('',*,*,#7333,.T.);
#9729=ORIENTED_EDGE('',*,*,#7334,.T.);
#9730=ORIENTED_EDGE('',*,*,#7322,.T.);
#9731=ORIENTED_EDGE('',*,*,#7335,.T.);
#9732=ORIENTED_EDGE('',*,*,#7332,.F.);
#9733=ORIENTED_EDGE('',*,*,#7336,.T.);
#9734=ORIENTED_EDGE('',*,*,#7330,.F.);
#9735=ORIENTED_EDGE('',*,*,#7337,.T.);
#9736=ORIENTED_EDGE('',*,*,#7338,.T.);
#9737=ORIENTED_EDGE('',*,*,#7334,.F.);
#9738=ORIENTED_EDGE('',*,*,#7339,.T.);
#9739=ORIENTED_EDGE('',*,*,#7340,.T.);
#9740=ORIENTED_EDGE('',*,*,#7341,.T.);
#9741=ORIENTED_EDGE('',*,*,#7328,.F.);
#9742=ORIENTED_EDGE('',*,*,#7314,.F.);
#9743=ORIENTED_EDGE('',*,*,#7342,.F.);
#9744=ORIENTED_EDGE('',*,*,#7343,.F.);
#9745=ORIENTED_EDGE('',*,*,#7340,.F.);
#9746=ORIENTED_EDGE('',*,*,#7344,.F.);
#9747=ORIENTED_EDGE('',*,*,#7325,.F.);
#9748=ORIENTED_EDGE('',*,*,#7333,.F.);
#9749=ORIENTED_EDGE('',*,*,#7335,.F.);
#9750=ORIENTED_EDGE('',*,*,#7321,.T.);
#9751=ORIENTED_EDGE('',*,*,#7326,.T.);
#9752=ORIENTED_EDGE('',*,*,#7344,.T.);
#9753=ORIENTED_EDGE('',*,*,#7339,.F.);
#9754=ORIENTED_EDGE('',*,*,#7345,.F.);
#9755=ORIENTED_EDGE('',*,*,#7225,.F.);
#9756=ORIENTED_EDGE('',*,*,#7346,.F.);
#9757=ORIENTED_EDGE('',*,*,#7149,.T.);
#9758=ORIENTED_EDGE('',*,*,#7331,.F.);
#9759=ORIENTED_EDGE('',*,*,#7338,.F.);
#9760=ORIENTED_EDGE('',*,*,#7327,.F.);
#9761=ORIENTED_EDGE('',*,*,#7336,.F.);
#9762=ORIENTED_EDGE('',*,*,#7226,.T.);
#9763=ORIENTED_EDGE('',*,*,#7345,.T.);
#9764=ORIENTED_EDGE('',*,*,#7148,.T.);
#9765=ORIENTED_EDGE('',*,*,#7144,.F.);
#9766=ORIENTED_EDGE('',*,*,#7214,.T.);
#9767=ORIENTED_EDGE('',*,*,#7221,.F.);
#9768=ORIENTED_EDGE('',*,*,#7293,.F.);
#9769=ORIENTED_EDGE('',*,*,#7307,.F.);
#9770=ORIENTED_EDGE('',*,*,#7216,.F.);
#9771=ORIENTED_EDGE('',*,*,#7295,.F.);
#9772=ORIENTED_EDGE('',*,*,#7347,.T.);
#9773=ORIENTED_EDGE('',*,*,#7224,.T.);
#9774=ORIENTED_EDGE('',*,*,#7278,.F.);
#9775=ORIENTED_EDGE('',*,*,#7189,.T.);
#9776=ORIENTED_EDGE('',*,*,#7290,.F.);
#9777=ORIENTED_EDGE('',*,*,#7150,.T.);
#9778=ORIENTED_EDGE('',*,*,#7346,.T.);
#9779=ORIENTED_EDGE('',*,*,#7329,.F.);
#9780=ORIENTED_EDGE('',*,*,#7341,.F.);
#9781=ORIENTED_EDGE('',*,*,#7343,.T.);
#9782=ORIENTED_EDGE('',*,*,#7348,.F.);
#9783=ORIENTED_EDGE('',*,*,#7323,.T.);
#9784=ORIENTED_EDGE('',*,*,#7337,.F.);
#9785=ORIENTED_EDGE('',*,*,#7309,.F.);
#9786=ORIENTED_EDGE('',*,*,#7319,.F.);
#9787=ORIENTED_EDGE('',*,*,#7324,.T.);
#9788=ORIENTED_EDGE('',*,*,#7348,.T.);
#9789=ORIENTED_EDGE('',*,*,#7342,.T.);
#9790=ORIENTED_EDGE('',*,*,#7316,.F.);
#9791=ORIENTED_EDGE('',*,*,#7253,.F.);
#9792=ORIENTED_EDGE('',*,*,#7349,.T.);
#9793=ORIENTED_EDGE('',*,*,#7273,.F.);
#9794=ORIENTED_EDGE('',*,*,#7349,.F.);
#9795=ORIENTED_EDGE('',*,*,#7347,.F.);
#9796=ORIENTED_EDGE('',*,*,#7350,.T.);
#9797=ORIENTED_EDGE('',*,*,#7351,.F.);
#9798=ORIENTED_EDGE('',*,*,#7350,.F.);
#9799=ORIENTED_EDGE('',*,*,#7352,.F.);
#9800=ORIENTED_EDGE('',*,*,#7353,.T.);
#9801=ORIENTED_EDGE('',*,*,#7147,.F.);
#9802=ORIENTED_EDGE('',*,*,#7353,.F.);
#9803=ORIENTED_EDGE('',*,*,#7274,.F.);
#9804=ORIENTED_EDGE('',*,*,#7354,.T.);
#9805=ORIENTED_EDGE('',*,*,#7289,.F.);
#9806=ORIENTED_EDGE('',*,*,#7354,.F.);
#9807=ORIENTED_EDGE('',*,*,#7269,.F.);
#9808=ORIENTED_EDGE('',*,*,#7192,.T.);
#9809=ORIENTED_EDGE('',*,*,#7280,.F.);
#9810=ORIENTED_EDGE('',*,*,#7355,.T.);
#9811=ORIENTED_EDGE('',*,*,#7263,.F.);
#9812=ORIENTED_EDGE('',*,*,#7356,.T.);
#9813=ORIENTED_EDGE('',*,*,#7286,.F.);
#9814=ORIENTED_EDGE('',*,*,#7211,.T.);
#9815=ORIENTED_EDGE('',*,*,#7164,.F.);
#9816=ORIENTED_EDGE('',*,*,#7299,.T.);
#9817=ORIENTED_EDGE('',*,*,#7181,.F.);
#9818=ORIENTED_EDGE('',*,*,#7357,.T.);
#9819=ORIENTED_EDGE('',*,*,#7162,.F.);
#9820=ORIENTED_EDGE('',*,*,#7357,.F.);
#9821=ORIENTED_EDGE('',*,*,#7152,.F.);
#9822=ORIENTED_EDGE('',*,*,#7358,.F.);
#9823=ORIENTED_EDGE('',*,*,#7351,.T.);
#9824=ORIENTED_EDGE('',*,*,#7267,.F.);
#9825=ORIENTED_EDGE('',*,*,#7355,.F.);
#9826=ORIENTED_EDGE('',*,*,#7283,.F.);
#9827=ORIENTED_EDGE('',*,*,#7356,.F.);
#9828=ORIENTED_EDGE('',*,*,#7156,.F.);
#9829=ORIENTED_EDGE('',*,*,#7358,.T.);
#9830=ORIENTED_EDGE('',*,*,#7180,.F.);
#9831=ORIENTED_EDGE('',*,*,#7178,.F.);
#9832=ORIENTED_EDGE('',*,*,#7175,.F.);
#9833=ORIENTED_EDGE('',*,*,#7172,.F.);
#9834=ORIENTED_EDGE('',*,*,#7352,.T.);
#9835=ORIENTED_EDGE('',*,*,#7359,.T.);
#9836=ORIENTED_EDGE('',*,*,#7360,.T.);
#9837=ORIENTED_EDGE('',*,*,#7361,.T.);
#9838=ORIENTED_EDGE('',*,*,#7362,.T.);
#9839=ORIENTED_EDGE('',*,*,#7363,.T.);
#9840=ORIENTED_EDGE('',*,*,#7364,.T.);
#9841=ORIENTED_EDGE('',*,*,#7361,.F.);
#9842=ORIENTED_EDGE('',*,*,#7365,.T.);
#9843=ORIENTED_EDGE('',*,*,#7366,.T.);
#9844=ORIENTED_EDGE('',*,*,#7367,.T.);
#9845=ORIENTED_EDGE('',*,*,#7363,.F.);
#9846=ORIENTED_EDGE('',*,*,#7368,.T.);
#9847=ORIENTED_EDGE('',*,*,#7368,.F.);
#9848=ORIENTED_EDGE('',*,*,#7369,.F.);
#9849=ORIENTED_EDGE('',*,*,#7370,.F.);
#9850=ORIENTED_EDGE('',*,*,#7371,.F.);
#9851=ORIENTED_EDGE('',*,*,#7365,.F.);
#9852=ORIENTED_EDGE('',*,*,#7372,.F.);
#9853=ORIENTED_EDGE('',*,*,#7373,.F.);
#9854=ORIENTED_EDGE('',*,*,#7369,.T.);
#9855=ORIENTED_EDGE('',*,*,#7360,.F.);
#9856=ORIENTED_EDGE('',*,*,#7374,.F.);
#9857=ORIENTED_EDGE('',*,*,#7375,.F.);
#9858=ORIENTED_EDGE('',*,*,#7372,.T.);
#9859=ORIENTED_EDGE('',*,*,#7376,.T.);
#9860=ORIENTED_EDGE('',*,*,#7377,.T.);
#9861=ORIENTED_EDGE('',*,*,#7378,.T.);
#9862=ORIENTED_EDGE('',*,*,#7375,.T.);
#9863=ORIENTED_EDGE('',*,*,#7379,.T.);
#9864=ORIENTED_EDGE('',*,*,#7373,.T.);
#9865=ORIENTED_EDGE('',*,*,#7378,.F.);
#9866=ORIENTED_EDGE('',*,*,#7380,.T.);
#9867=ORIENTED_EDGE('',*,*,#7381,.T.);
#9868=ORIENTED_EDGE('',*,*,#7370,.T.);
#9869=ORIENTED_EDGE('',*,*,#7379,.F.);
#9870=ORIENTED_EDGE('',*,*,#7382,.T.);
#9871=ORIENTED_EDGE('',*,*,#7382,.F.);
#9872=ORIENTED_EDGE('',*,*,#7380,.F.);
#9873=ORIENTED_EDGE('',*,*,#7377,.F.);
#9874=ORIENTED_EDGE('',*,*,#7383,.F.);
#9875=ORIENTED_EDGE('',*,*,#7384,.F.);
#9876=ORIENTED_EDGE('',*,*,#7385,.F.);
#9877=ORIENTED_EDGE('',*,*,#7386,.F.);
#9878=ORIENTED_EDGE('',*,*,#7387,.F.);
#9879=ORIENTED_EDGE('',*,*,#7388,.F.);
#9880=ORIENTED_EDGE('',*,*,#7389,.F.);
#9881=ORIENTED_EDGE('',*,*,#7390,.T.);
#9882=ORIENTED_EDGE('',*,*,#7391,.T.);
#9883=ORIENTED_EDGE('',*,*,#7392,.T.);
#9884=ORIENTED_EDGE('',*,*,#7393,.T.);
#9885=ORIENTED_EDGE('',*,*,#7394,.T.);
#9886=ORIENTED_EDGE('',*,*,#7395,.T.);
#9887=ORIENTED_EDGE('',*,*,#7392,.F.);
#9888=ORIENTED_EDGE('',*,*,#7396,.T.);
#9889=ORIENTED_EDGE('',*,*,#7397,.T.);
#9890=ORIENTED_EDGE('',*,*,#7398,.T.);
#9891=ORIENTED_EDGE('',*,*,#7394,.F.);
#9892=ORIENTED_EDGE('',*,*,#7399,.T.);
#9893=ORIENTED_EDGE('',*,*,#7399,.F.);
#9894=ORIENTED_EDGE('',*,*,#7400,.F.);
#9895=ORIENTED_EDGE('',*,*,#7401,.F.);
#9896=ORIENTED_EDGE('',*,*,#7402,.F.);
#9897=ORIENTED_EDGE('',*,*,#7396,.F.);
#9898=ORIENTED_EDGE('',*,*,#7403,.F.);
#9899=ORIENTED_EDGE('',*,*,#7404,.F.);
#9900=ORIENTED_EDGE('',*,*,#7400,.T.);
#9901=ORIENTED_EDGE('',*,*,#7391,.F.);
#9902=ORIENTED_EDGE('',*,*,#7405,.F.);
#9903=ORIENTED_EDGE('',*,*,#7406,.F.);
#9904=ORIENTED_EDGE('',*,*,#7403,.T.);
#9905=ORIENTED_EDGE('',*,*,#7407,.F.);
#9906=ORIENTED_EDGE('',*,*,#7408,.F.);
#9907=ORIENTED_EDGE('',*,*,#7409,.F.);
#9908=ORIENTED_EDGE('',*,*,#7410,.T.);
#9909=ORIENTED_EDGE('',*,*,#7411,.T.);
#9910=ORIENTED_EDGE('',*,*,#7408,.T.);
#9911=ORIENTED_EDGE('',*,*,#7412,.T.);
#9912=ORIENTED_EDGE('',*,*,#7413,.T.);
#9913=ORIENTED_EDGE('',*,*,#7414,.T.);
#9914=ORIENTED_EDGE('',*,*,#7409,.T.);
#9915=ORIENTED_EDGE('',*,*,#7415,.T.);
#9916=ORIENTED_EDGE('',*,*,#7416,.T.);
#9917=ORIENTED_EDGE('',*,*,#7417,.T.);
#9918=ORIENTED_EDGE('',*,*,#7418,.T.);
#9919=ORIENTED_EDGE('',*,*,#7407,.T.);
#9920=ORIENTED_EDGE('',*,*,#7419,.T.);
#9921=ORIENTED_EDGE('',*,*,#7420,.T.);
#9922=ORIENTED_EDGE('',*,*,#7415,.F.);
#9923=ORIENTED_EDGE('',*,*,#7411,.F.);
#9924=ORIENTED_EDGE('',*,*,#7421,.F.);
#9925=ORIENTED_EDGE('',*,*,#7422,.F.);
#9926=ORIENTED_EDGE('',*,*,#7412,.F.);
#9927=ORIENTED_EDGE('',*,*,#7418,.F.);
#9928=ORIENTED_EDGE('',*,*,#7423,.F.);
#9929=ORIENTED_EDGE('',*,*,#7424,.F.);
#9930=ORIENTED_EDGE('',*,*,#7417,.F.);
#9931=ORIENTED_EDGE('',*,*,#7425,.T.);
#9932=ORIENTED_EDGE('',*,*,#7426,.T.);
#9933=ORIENTED_EDGE('',*,*,#7427,.T.);
#9934=ORIENTED_EDGE('',*,*,#7423,.T.);
#9935=ORIENTED_EDGE('',*,*,#7428,.T.);
#9936=ORIENTED_EDGE('',*,*,#7429,.T.);
#9937=ORIENTED_EDGE('',*,*,#7430,.T.);
#9938=ORIENTED_EDGE('',*,*,#7429,.F.);
#9939=ORIENTED_EDGE('',*,*,#7430,.F.);
#9940=ORIENTED_EDGE('',*,*,#7431,.T.);
#9941=ORIENTED_EDGE('',*,*,#7432,.F.);
#9942=ORIENTED_EDGE('',*,*,#7431,.F.);
#9943=ORIENTED_EDGE('',*,*,#7367,.F.);
#9944=ORIENTED_EDGE('',*,*,#7433,.F.);
#9945=ORIENTED_EDGE('',*,*,#7362,.F.);
#9946=ORIENTED_EDGE('',*,*,#7364,.F.);
#9947=ORIENTED_EDGE('',*,*,#7428,.F.);
#9948=ORIENTED_EDGE('',*,*,#7434,.T.);
#9949=ORIENTED_EDGE('',*,*,#7435,.T.);
#9950=ORIENTED_EDGE('',*,*,#7436,.T.);
#9951=ORIENTED_EDGE('',*,*,#7435,.F.);
#9952=ORIENTED_EDGE('',*,*,#7436,.F.);
#9953=ORIENTED_EDGE('',*,*,#7437,.T.);
#9954=ORIENTED_EDGE('',*,*,#7438,.F.);
#9955=ORIENTED_EDGE('',*,*,#7437,.F.);
#9956=ORIENTED_EDGE('',*,*,#7398,.F.);
#9957=ORIENTED_EDGE('',*,*,#7439,.F.);
#9958=ORIENTED_EDGE('',*,*,#7393,.F.);
#9959=ORIENTED_EDGE('',*,*,#7395,.F.);
#9960=ORIENTED_EDGE('',*,*,#7434,.F.);
#9961=ORIENTED_EDGE('',*,*,#7432,.T.);
#9962=ORIENTED_EDGE('',*,*,#7440,.T.);
#9963=ORIENTED_EDGE('',*,*,#7441,.T.);
#9964=ORIENTED_EDGE('',*,*,#7440,.F.);
#9965=ORIENTED_EDGE('',*,*,#7442,.F.);
#9966=ORIENTED_EDGE('',*,*,#7443,.F.);
#9967=ORIENTED_EDGE('',*,*,#7444,.F.);
#9968=ORIENTED_EDGE('',*,*,#7445,.F.);
#9969=ORIENTED_EDGE('',*,*,#7446,.F.);
#9970=ORIENTED_EDGE('',*,*,#7447,.F.);
#9971=ORIENTED_EDGE('',*,*,#7441,.F.);
#9972=ORIENTED_EDGE('',*,*,#7387,.T.);
#9973=ORIENTED_EDGE('',*,*,#7448,.T.);
#9974=ORIENTED_EDGE('',*,*,#7449,.T.);
#9975=ORIENTED_EDGE('',*,*,#7450,.F.);
#9976=ORIENTED_EDGE('',*,*,#7386,.T.);
#9977=ORIENTED_EDGE('',*,*,#7451,.T.);
#9978=ORIENTED_EDGE('',*,*,#7452,.T.);
#9979=ORIENTED_EDGE('',*,*,#7448,.F.);
#9980=ORIENTED_EDGE('',*,*,#7384,.T.);
#9981=ORIENTED_EDGE('',*,*,#7453,.T.);
#9982=ORIENTED_EDGE('',*,*,#7454,.T.);
#9983=ORIENTED_EDGE('',*,*,#7455,.T.);
#9984=ORIENTED_EDGE('',*,*,#7456,.T.);
#9985=ORIENTED_EDGE('',*,*,#7453,.F.);
#9986=ORIENTED_EDGE('',*,*,#7389,.T.);
#9987=ORIENTED_EDGE('',*,*,#7457,.T.);
#9988=ORIENTED_EDGE('',*,*,#7385,.T.);
#9989=ORIENTED_EDGE('',*,*,#7455,.F.);
#9990=ORIENTED_EDGE('',*,*,#7458,.T.);
#9991=ORIENTED_EDGE('',*,*,#7451,.F.);
#9992=ORIENTED_EDGE('',*,*,#7459,.T.);
#9993=ORIENTED_EDGE('',*,*,#7457,.F.);
#9994=ORIENTED_EDGE('',*,*,#7388,.T.);
#9995=ORIENTED_EDGE('',*,*,#7450,.T.);
#9996=ORIENTED_EDGE('',*,*,#7452,.F.);
#9997=ORIENTED_EDGE('',*,*,#7460,.T.);
#9998=ORIENTED_EDGE('',*,*,#7447,.T.);
#9999=ORIENTED_EDGE('',*,*,#7461,.F.);
#10000=ORIENTED_EDGE('',*,*,#7458,.F.);
#10001=ORIENTED_EDGE('',*,*,#7462,.T.);
#10002=ORIENTED_EDGE('',*,*,#7442,.T.);
#10003=ORIENTED_EDGE('',*,*,#7460,.F.);
#10004=ORIENTED_EDGE('',*,*,#7454,.F.);
#10005=ORIENTED_EDGE('',*,*,#7463,.T.);
#10006=ORIENTED_EDGE('',*,*,#7443,.T.);
#10007=ORIENTED_EDGE('',*,*,#7462,.F.);
#10008=ORIENTED_EDGE('',*,*,#7438,.T.);
#10009=ORIENTED_EDGE('',*,*,#7464,.T.);
#10010=ORIENTED_EDGE('',*,*,#7465,.T.);
#10011=ORIENTED_EDGE('',*,*,#7464,.F.);
#10012=ORIENTED_EDGE('',*,*,#7466,.F.);
#10013=ORIENTED_EDGE('',*,*,#7467,.F.);
#10014=ORIENTED_EDGE('',*,*,#7468,.F.);
#10015=ORIENTED_EDGE('',*,*,#7469,.F.);
#10016=ORIENTED_EDGE('',*,*,#7470,.F.);
#10017=ORIENTED_EDGE('',*,*,#7471,.F.);
#10018=ORIENTED_EDGE('',*,*,#7465,.F.);
#10019=ORIENTED_EDGE('',*,*,#7472,.T.);
#10020=ORIENTED_EDGE('',*,*,#7401,.T.);
#10021=ORIENTED_EDGE('',*,*,#7473,.T.);
#10022=ORIENTED_EDGE('',*,*,#7474,.T.);
#10023=ORIENTED_EDGE('',*,*,#7475,.T.);
#10024=ORIENTED_EDGE('',*,*,#7476,.T.);
#10025=ORIENTED_EDGE('',*,*,#7473,.F.);
#10026=ORIENTED_EDGE('',*,*,#7404,.T.);
#10027=ORIENTED_EDGE('',*,*,#7477,.T.);
#10028=ORIENTED_EDGE('',*,*,#7478,.T.);
#10029=ORIENTED_EDGE('',*,*,#7475,.F.);
#10030=ORIENTED_EDGE('',*,*,#7406,.T.);
#10031=ORIENTED_EDGE('',*,*,#7479,.T.);
#10032=ORIENTED_EDGE('',*,*,#7480,.T.);
#10033=ORIENTED_EDGE('',*,*,#7481,.T.);
#10034=ORIENTED_EDGE('',*,*,#7482,.F.);
#10035=ORIENTED_EDGE('',*,*,#7483,.T.);
#10036=ORIENTED_EDGE('',*,*,#7484,.T.);
#10037=ORIENTED_EDGE('',*,*,#7485,.T.);
#10038=ORIENTED_EDGE('',*,*,#7480,.F.);
#10039=ORIENTED_EDGE('',*,*,#7486,.T.);
#10040=ORIENTED_EDGE('',*,*,#7487,.T.);
#10041=ORIENTED_EDGE('',*,*,#7488,.T.);
#10042=ORIENTED_EDGE('',*,*,#7489,.T.);
#10043=ORIENTED_EDGE('',*,*,#7490,.T.);
#10044=ORIENTED_EDGE('',*,*,#7487,.F.);
#10045=ORIENTED_EDGE('',*,*,#7491,.T.);
#10046=ORIENTED_EDGE('',*,*,#7492,.T.);
#10047=ORIENTED_EDGE('',*,*,#7493,.T.);
#10048=ORIENTED_EDGE('',*,*,#7489,.F.);
#10049=ORIENTED_EDGE('',*,*,#7494,.T.);
#10050=ORIENTED_EDGE('',*,*,#7484,.F.);
#10051=ORIENTED_EDGE('',*,*,#7495,.T.);
#10052=ORIENTED_EDGE('',*,*,#7492,.F.);
#10053=ORIENTED_EDGE('',*,*,#7496,.T.);
#10054=ORIENTED_EDGE('',*,*,#7482,.T.);
#10055=ORIENTED_EDGE('',*,*,#7485,.F.);
#10056=ORIENTED_EDGE('',*,*,#7497,.T.);
#10057=ORIENTED_EDGE('',*,*,#7471,.T.);
#10058=ORIENTED_EDGE('',*,*,#7498,.F.);
#10059=ORIENTED_EDGE('',*,*,#7494,.F.);
#10060=ORIENTED_EDGE('',*,*,#7499,.T.);
#10061=ORIENTED_EDGE('',*,*,#7466,.T.);
#10062=ORIENTED_EDGE('',*,*,#7497,.F.);
#10063=ORIENTED_EDGE('',*,*,#7488,.F.);
#10064=ORIENTED_EDGE('',*,*,#7500,.T.);
#10065=ORIENTED_EDGE('',*,*,#7467,.T.);
#10066=ORIENTED_EDGE('',*,*,#7499,.F.);
#10067=ORIENTED_EDGE('',*,*,#7478,.F.);
#10068=ORIENTED_EDGE('',*,*,#7501,.F.);
#10069=ORIENTED_EDGE('',*,*,#7474,.F.);
#10070=ORIENTED_EDGE('',*,*,#7476,.F.);
#10071=ORIENTED_EDGE('',*,*,#7486,.F.);
#10072=ORIENTED_EDGE('',*,*,#7493,.F.);
#10073=ORIENTED_EDGE('',*,*,#7483,.F.);
#10074=ORIENTED_EDGE('',*,*,#7479,.F.);
#10075=ORIENTED_EDGE('',*,*,#7496,.F.);
#10076=ORIENTED_EDGE('',*,*,#7491,.F.);
#10077=ORIENTED_EDGE('',*,*,#7502,.F.);
#10078=ORIENTED_EDGE('',*,*,#7503,.F.);
#10079=ORIENTED_EDGE('',*,*,#7504,.F.);
#10080=ORIENTED_EDGE('',*,*,#7505,.T.);
#10081=ORIENTED_EDGE('',*,*,#7506,.T.);
#10082=ORIENTED_EDGE('',*,*,#7503,.T.);
#10083=ORIENTED_EDGE('',*,*,#7507,.T.);
#10084=ORIENTED_EDGE('',*,*,#7508,.F.);
#10085=ORIENTED_EDGE('',*,*,#7509,.F.);
#10086=ORIENTED_EDGE('',*,*,#7510,.F.);
#10087=ORIENTED_EDGE('',*,*,#7511,.T.);
#10088=ORIENTED_EDGE('',*,*,#7512,.T.);
#10089=ORIENTED_EDGE('',*,*,#7509,.T.);
#10090=ORIENTED_EDGE('',*,*,#7513,.T.);
#10091=ORIENTED_EDGE('',*,*,#7514,.T.);
#10092=ORIENTED_EDGE('',*,*,#7515,.T.);
#10093=ORIENTED_EDGE('',*,*,#7510,.T.);
#10094=ORIENTED_EDGE('',*,*,#7516,.T.);
#10095=ORIENTED_EDGE('',*,*,#7517,.T.);
#10096=ORIENTED_EDGE('',*,*,#7508,.T.);
#10097=ORIENTED_EDGE('',*,*,#7518,.T.);
#10098=ORIENTED_EDGE('',*,*,#7504,.T.);
#10099=ORIENTED_EDGE('',*,*,#7519,.T.);
#10100=ORIENTED_EDGE('',*,*,#7520,.T.);
#10101=ORIENTED_EDGE('',*,*,#7521,.T.);
#10102=ORIENTED_EDGE('',*,*,#7502,.T.);
#10103=ORIENTED_EDGE('',*,*,#7522,.T.);
#10104=ORIENTED_EDGE('',*,*,#7523,.T.);
#10105=ORIENTED_EDGE('',*,*,#7513,.F.);
#10106=ORIENTED_EDGE('',*,*,#7519,.F.);
#10107=ORIENTED_EDGE('',*,*,#7506,.F.);
#10108=ORIENTED_EDGE('',*,*,#7524,.F.);
#10109=ORIENTED_EDGE('',*,*,#7507,.F.);
#10110=ORIENTED_EDGE('',*,*,#7521,.F.);
#10111=ORIENTED_EDGE('',*,*,#7525,.F.);
#10112=ORIENTED_EDGE('',*,*,#7526,.F.);
#10113=ORIENTED_EDGE('',*,*,#7520,.F.);
#10114=ORIENTED_EDGE('',*,*,#7527,.T.);
#10115=ORIENTED_EDGE('',*,*,#7528,.T.);
#10116=ORIENTED_EDGE('',*,*,#7529,.F.);
#10117=ORIENTED_EDGE('',*,*,#7525,.T.);
#10118=ORIENTED_EDGE('',*,*,#7530,.F.);
#10119=ORIENTED_EDGE('',*,*,#7531,.F.);
#10120=ORIENTED_EDGE('',*,*,#7532,.F.);
#10121=ORIENTED_EDGE('',*,*,#7533,.T.);
#10122=ORIENTED_EDGE('',*,*,#7534,.T.);
#10123=ORIENTED_EDGE('',*,*,#7531,.T.);
#10124=ORIENTED_EDGE('',*,*,#7535,.T.);
#10125=ORIENTED_EDGE('',*,*,#7536,.F.);
#10126=ORIENTED_EDGE('',*,*,#7537,.F.);
#10127=ORIENTED_EDGE('',*,*,#7538,.F.);
#10128=ORIENTED_EDGE('',*,*,#7539,.T.);
#10129=ORIENTED_EDGE('',*,*,#7540,.T.);
#10130=ORIENTED_EDGE('',*,*,#7537,.T.);
#10131=ORIENTED_EDGE('',*,*,#7541,.T.);
#10132=ORIENTED_EDGE('',*,*,#7542,.T.);
#10133=ORIENTED_EDGE('',*,*,#7543,.T.);
#10134=ORIENTED_EDGE('',*,*,#7538,.T.);
#10135=ORIENTED_EDGE('',*,*,#7544,.T.);
#10136=ORIENTED_EDGE('',*,*,#7545,.T.);
#10137=ORIENTED_EDGE('',*,*,#7536,.T.);
#10138=ORIENTED_EDGE('',*,*,#7546,.T.);
#10139=ORIENTED_EDGE('',*,*,#7532,.T.);
#10140=ORIENTED_EDGE('',*,*,#7547,.T.);
#10141=ORIENTED_EDGE('',*,*,#7548,.T.);
#10142=ORIENTED_EDGE('',*,*,#7549,.T.);
#10143=ORIENTED_EDGE('',*,*,#7530,.T.);
#10144=ORIENTED_EDGE('',*,*,#7550,.T.);
#10145=ORIENTED_EDGE('',*,*,#7551,.T.);
#10146=ORIENTED_EDGE('',*,*,#7541,.F.);
#10147=ORIENTED_EDGE('',*,*,#7547,.F.);
#10148=ORIENTED_EDGE('',*,*,#7534,.F.);
#10149=ORIENTED_EDGE('',*,*,#7552,.F.);
#10150=ORIENTED_EDGE('',*,*,#7535,.F.);
#10151=ORIENTED_EDGE('',*,*,#7549,.F.);
#10152=ORIENTED_EDGE('',*,*,#7553,.F.);
#10153=ORIENTED_EDGE('',*,*,#7554,.F.);
#10154=ORIENTED_EDGE('',*,*,#7548,.F.);
#10155=ORIENTED_EDGE('',*,*,#7555,.T.);
#10156=ORIENTED_EDGE('',*,*,#7556,.T.);
#10157=ORIENTED_EDGE('',*,*,#7557,.F.);
#10158=ORIENTED_EDGE('',*,*,#7553,.T.);
#10159=ORIENTED_EDGE('',*,*,#7420,.F.);
#10160=ORIENTED_EDGE('',*,*,#7558,.T.);
#10161=ORIENTED_EDGE('',*,*,#7559,.T.);
#10162=ORIENTED_EDGE('',*,*,#7560,.T.);
#10163=ORIENTED_EDGE('',*,*,#7561,.T.);
#10164=ORIENTED_EDGE('',*,*,#7425,.F.);
#10165=ORIENTED_EDGE('',*,*,#7426,.F.);
#10166=ORIENTED_EDGE('',*,*,#7561,.F.);
#10167=ORIENTED_EDGE('',*,*,#7562,.F.);
#10168=ORIENTED_EDGE('',*,*,#7563,.F.);
#10169=ORIENTED_EDGE('',*,*,#7560,.F.);
#10170=ORIENTED_EDGE('',*,*,#7564,.T.);
#10171=ORIENTED_EDGE('',*,*,#7565,.T.);
#10172=ORIENTED_EDGE('',*,*,#7566,.F.);
#10173=ORIENTED_EDGE('',*,*,#7562,.T.);
#10174=ORIENTED_EDGE('',*,*,#7567,.T.);
#10175=ORIENTED_EDGE('',*,*,#7568,.T.);
#10176=ORIENTED_EDGE('',*,*,#7569,.T.);
#10177=ORIENTED_EDGE('',*,*,#7570,.T.);
#10178=ORIENTED_EDGE('',*,*,#7571,.T.);
#10179=ORIENTED_EDGE('',*,*,#7572,.T.);
#10180=ORIENTED_EDGE('',*,*,#7573,.T.);
#10181=ORIENTED_EDGE('',*,*,#7570,.F.);
#10182=ORIENTED_EDGE('',*,*,#7567,.F.);
#10183=ORIENTED_EDGE('',*,*,#7574,.T.);
#10184=ORIENTED_EDGE('',*,*,#7575,.T.);
#10185=ORIENTED_EDGE('',*,*,#7576,.F.);
#10186=ORIENTED_EDGE('',*,*,#7573,.F.);
#10187=ORIENTED_EDGE('',*,*,#7577,.T.);
#10188=ORIENTED_EDGE('',*,*,#7578,.T.);
#10189=ORIENTED_EDGE('',*,*,#7574,.F.);
#10190=ORIENTED_EDGE('',*,*,#7579,.T.);
#10191=ORIENTED_EDGE('',*,*,#7568,.F.);
#10192=ORIENTED_EDGE('',*,*,#7580,.T.);
#10193=ORIENTED_EDGE('',*,*,#7581,.T.);
#10194=ORIENTED_EDGE('',*,*,#7582,.T.);
#10195=ORIENTED_EDGE('',*,*,#7572,.F.);
#10196=ORIENTED_EDGE('',*,*,#7583,.T.);
#10197=ORIENTED_EDGE('',*,*,#7581,.F.);
#10198=ORIENTED_EDGE('',*,*,#7584,.F.);
#10199=ORIENTED_EDGE('',*,*,#7585,.F.);
#10200=ORIENTED_EDGE('',*,*,#7586,.F.);
#10201=ORIENTED_EDGE('',*,*,#7587,.F.);
#10202=ORIENTED_EDGE('',*,*,#7588,.F.);
#10203=ORIENTED_EDGE('',*,*,#7528,.F.);
#10204=ORIENTED_EDGE('',*,*,#7589,.F.);
#10205=ORIENTED_EDGE('',*,*,#7590,.F.);
#10206=ORIENTED_EDGE('',*,*,#7591,.F.);
#10207=ORIENTED_EDGE('',*,*,#7556,.F.);
#10208=ORIENTED_EDGE('',*,*,#7592,.F.);
#10209=ORIENTED_EDGE('',*,*,#7593,.F.);
#10210=ORIENTED_EDGE('',*,*,#7594,.F.);
#10211=ORIENTED_EDGE('',*,*,#7565,.F.);
#10212=ORIENTED_EDGE('',*,*,#7595,.F.);
#10213=ORIENTED_EDGE('',*,*,#7596,.F.);
#10214=ORIENTED_EDGE('',*,*,#7597,.F.);
#10215=ORIENTED_EDGE('',*,*,#7598,.F.);
#10216=ORIENTED_EDGE('',*,*,#7599,.F.);
#10217=ORIENTED_EDGE('',*,*,#7600,.F.);
#10218=ORIENTED_EDGE('',*,*,#7579,.F.);
#10219=ORIENTED_EDGE('',*,*,#7583,.F.);
#10220=ORIENTED_EDGE('',*,*,#7571,.F.);
#10221=ORIENTED_EDGE('',*,*,#7569,.F.);
#10222=ORIENTED_EDGE('',*,*,#7601,.T.);
#10223=ORIENTED_EDGE('',*,*,#7584,.T.);
#10224=ORIENTED_EDGE('',*,*,#7602,.T.);
#10225=ORIENTED_EDGE('',*,*,#7603,.T.);
#10226=ORIENTED_EDGE('',*,*,#7604,.T.);
#10227=ORIENTED_EDGE('',*,*,#7605,.T.);
#10228=ORIENTED_EDGE('',*,*,#7601,.F.);
#10229=ORIENTED_EDGE('',*,*,#7606,.T.);
#10230=ORIENTED_EDGE('',*,*,#7607,.T.);
#10231=ORIENTED_EDGE('',*,*,#7608,.T.);
#10232=ORIENTED_EDGE('',*,*,#7604,.F.);
#10233=ORIENTED_EDGE('',*,*,#7609,.T.);
#10234=ORIENTED_EDGE('',*,*,#7610,.T.);
#10235=ORIENTED_EDGE('',*,*,#7611,.T.);
#10236=ORIENTED_EDGE('',*,*,#7607,.F.);
#10237=ORIENTED_EDGE('',*,*,#7612,.T.);
#10238=ORIENTED_EDGE('',*,*,#7613,.T.);
#10239=ORIENTED_EDGE('',*,*,#7614,.T.);
#10240=ORIENTED_EDGE('',*,*,#7610,.F.);
#10241=ORIENTED_EDGE('',*,*,#7615,.T.);
#10242=ORIENTED_EDGE('',*,*,#7616,.T.);
#10243=ORIENTED_EDGE('',*,*,#7617,.T.);
#10244=ORIENTED_EDGE('',*,*,#7613,.F.);
#10245=ORIENTED_EDGE('',*,*,#7618,.T.);
#10246=ORIENTED_EDGE('',*,*,#7619,.T.);
#10247=ORIENTED_EDGE('',*,*,#7620,.T.);
#10248=ORIENTED_EDGE('',*,*,#7616,.F.);
#10249=ORIENTED_EDGE('',*,*,#7621,.T.);
#10250=ORIENTED_EDGE('',*,*,#7602,.F.);
#10251=ORIENTED_EDGE('',*,*,#7622,.T.);
#10252=ORIENTED_EDGE('',*,*,#7619,.F.);
#10253=ORIENTED_EDGE('',*,*,#7623,.T.);
#10254=ORIENTED_EDGE('',*,*,#7617,.F.);
#10255=ORIENTED_EDGE('',*,*,#7624,.T.);
#10256=ORIENTED_EDGE('',*,*,#7625,.F.);
#10257=ORIENTED_EDGE('',*,*,#7626,.T.);
#10258=ORIENTED_EDGE('',*,*,#7620,.F.);
#10259=ORIENTED_EDGE('',*,*,#7627,.F.);
#10260=ORIENTED_EDGE('',*,*,#7628,.F.);
#10261=ORIENTED_EDGE('',*,*,#7624,.F.);
#10262=ORIENTED_EDGE('',*,*,#7629,.F.);
#10263=ORIENTED_EDGE('',*,*,#7622,.F.);
#10264=ORIENTED_EDGE('',*,*,#7600,.T.);
#10265=ORIENTED_EDGE('',*,*,#7630,.F.);
#10266=ORIENTED_EDGE('',*,*,#7631,.F.);
#10267=ORIENTED_EDGE('',*,*,#7632,.F.);
#10268=ORIENTED_EDGE('',*,*,#7598,.T.);
#10269=ORIENTED_EDGE('',*,*,#7633,.F.);
#10270=ORIENTED_EDGE('',*,*,#7627,.T.);
#10271=ORIENTED_EDGE('',*,*,#7603,.F.);
#10272=ORIENTED_EDGE('',*,*,#7623,.F.);
#10273=ORIENTED_EDGE('',*,*,#7621,.F.);
#10274=ORIENTED_EDGE('',*,*,#7618,.F.);
#10275=ORIENTED_EDGE('',*,*,#7615,.F.);
#10276=ORIENTED_EDGE('',*,*,#7612,.F.);
#10277=ORIENTED_EDGE('',*,*,#7609,.F.);
#10278=ORIENTED_EDGE('',*,*,#7606,.F.);
#10279=ORIENTED_EDGE('',*,*,#7634,.T.);
#10280=ORIENTED_EDGE('',*,*,#7566,.T.);
#10281=ORIENTED_EDGE('',*,*,#7594,.T.);
#10282=ORIENTED_EDGE('',*,*,#7635,.T.);
#10283=ORIENTED_EDGE('',*,*,#7591,.T.);
#10284=ORIENTED_EDGE('',*,*,#7636,.T.);
#10285=ORIENTED_EDGE('',*,*,#7637,.T.);
#10286=ORIENTED_EDGE('',*,*,#7557,.T.);
#10287=ORIENTED_EDGE('',*,*,#7517,.F.);
#10288=ORIENTED_EDGE('',*,*,#7638,.T.);
#10289=ORIENTED_EDGE('',*,*,#7636,.F.);
#10290=ORIENTED_EDGE('',*,*,#7590,.T.);
#10291=ORIENTED_EDGE('',*,*,#7639,.T.);
#10292=ORIENTED_EDGE('',*,*,#7588,.T.);
#10293=ORIENTED_EDGE('',*,*,#7640,.T.);
#10294=ORIENTED_EDGE('',*,*,#7641,.T.);
#10295=ORIENTED_EDGE('',*,*,#7529,.T.);
#10296=ORIENTED_EDGE('',*,*,#7640,.F.);
#10297=ORIENTED_EDGE('',*,*,#7642,.T.);
#10298=ORIENTED_EDGE('',*,*,#7643,.T.);
#10299=ORIENTED_EDGE('',*,*,#7644,.T.);
#10300=ORIENTED_EDGE('',*,*,#7645,.T.);
#10301=ORIENTED_EDGE('',*,*,#7646,.T.);
#10302=ORIENTED_EDGE('',*,*,#7643,.F.);
#10303=ORIENTED_EDGE('',*,*,#7647,.T.);
#10304=ORIENTED_EDGE('',*,*,#7645,.F.);
#10305=ORIENTED_EDGE('',*,*,#7648,.T.);
#10306=ORIENTED_EDGE('',*,*,#7649,.T.);
#10307=ORIENTED_EDGE('',*,*,#7650,.T.);
#10308=ORIENTED_EDGE('',*,*,#7651,.T.);
#10309=ORIENTED_EDGE('',*,*,#7652,.T.);
#10310=ORIENTED_EDGE('',*,*,#7649,.F.);
#10311=ORIENTED_EDGE('',*,*,#7653,.T.);
#10312=ORIENTED_EDGE('',*,*,#7651,.F.);
#10313=ORIENTED_EDGE('',*,*,#7625,.T.);
#10314=ORIENTED_EDGE('',*,*,#7654,.T.);
#10315=ORIENTED_EDGE('',*,*,#7655,.T.);
#10316=ORIENTED_EDGE('',*,*,#7656,.T.);
#10317=ORIENTED_EDGE('',*,*,#7657,.T.);
#10318=ORIENTED_EDGE('',*,*,#7654,.F.);
#10319=ORIENTED_EDGE('',*,*,#7628,.T.);
#10320=ORIENTED_EDGE('',*,*,#7656,.F.);
#10321=ORIENTED_EDGE('',*,*,#7633,.T.);
#10322=ORIENTED_EDGE('',*,*,#7658,.T.);
#10323=ORIENTED_EDGE('',*,*,#7659,.T.);
#10324=ORIENTED_EDGE('',*,*,#7660,.T.);
#10325=ORIENTED_EDGE('',*,*,#7658,.F.);
#10326=ORIENTED_EDGE('',*,*,#7597,.T.);
#10327=ORIENTED_EDGE('',*,*,#7661,.T.);
#10328=ORIENTED_EDGE('',*,*,#7416,.F.);
#10329=ORIENTED_EDGE('',*,*,#7422,.T.);
#10330=ORIENTED_EDGE('',*,*,#7661,.F.);
#10331=ORIENTED_EDGE('',*,*,#7596,.T.);
#10332=ORIENTED_EDGE('',*,*,#7662,.T.);
#10333=ORIENTED_EDGE('',*,*,#7514,.F.);
#10334=ORIENTED_EDGE('',*,*,#7639,.F.);
#10335=ORIENTED_EDGE('',*,*,#7589,.T.);
#10336=ORIENTED_EDGE('',*,*,#7527,.F.);
#10337=ORIENTED_EDGE('',*,*,#7523,.F.);
#10338=ORIENTED_EDGE('',*,*,#7663,.T.);
#10339=ORIENTED_EDGE('',*,*,#7413,.F.);
#10340=ORIENTED_EDGE('',*,*,#7662,.F.);
#10341=ORIENTED_EDGE('',*,*,#7595,.T.);
#10342=ORIENTED_EDGE('',*,*,#7564,.F.);
#10343=ORIENTED_EDGE('',*,*,#7559,.F.);
#10344=ORIENTED_EDGE('',*,*,#7664,.T.);
#10345=ORIENTED_EDGE('',*,*,#7545,.F.);
#10346=ORIENTED_EDGE('',*,*,#7665,.T.);
#10347=ORIENTED_EDGE('',*,*,#7635,.F.);
#10348=ORIENTED_EDGE('',*,*,#7593,.T.);
#10349=ORIENTED_EDGE('',*,*,#7666,.T.);
#10350=ORIENTED_EDGE('',*,*,#7542,.F.);
#10351=ORIENTED_EDGE('',*,*,#7666,.F.);
#10352=ORIENTED_EDGE('',*,*,#7592,.T.);
#10353=ORIENTED_EDGE('',*,*,#7555,.F.);
#10354=ORIENTED_EDGE('',*,*,#7551,.F.);
#10355=ORIENTED_EDGE('',*,*,#7667,.T.);
#10356=ORIENTED_EDGE('',*,*,#7614,.F.);
#10357=ORIENTED_EDGE('',*,*,#7626,.F.);
#10358=ORIENTED_EDGE('',*,*,#7653,.F.);
#10359=ORIENTED_EDGE('',*,*,#7668,.F.);
#10360=ORIENTED_EDGE('',*,*,#7611,.F.);
#10361=ORIENTED_EDGE('',*,*,#7668,.T.);
#10362=ORIENTED_EDGE('',*,*,#7648,.F.);
#10363=ORIENTED_EDGE('',*,*,#7669,.T.);
#10364=ORIENTED_EDGE('',*,*,#7608,.F.);
#10365=ORIENTED_EDGE('',*,*,#7669,.F.);
#10366=ORIENTED_EDGE('',*,*,#7647,.F.);
#10367=ORIENTED_EDGE('',*,*,#7670,.F.);
#10368=ORIENTED_EDGE('',*,*,#7605,.F.);
#10369=ORIENTED_EDGE('',*,*,#7670,.T.);
#10370=ORIENTED_EDGE('',*,*,#7642,.F.);
#10371=ORIENTED_EDGE('',*,*,#7587,.T.);
#10372=ORIENTED_EDGE('',*,*,#7671,.F.);
#10373=ORIENTED_EDGE('',*,*,#7672,.F.);
#10374=ORIENTED_EDGE('',*,*,#7673,.F.);
#10375=ORIENTED_EDGE('',*,*,#7585,.T.);
#10376=ORIENTED_EDGE('',*,*,#7540,.F.);
#10377=ORIENTED_EDGE('',*,*,#7674,.F.);
#10378=ORIENTED_EDGE('',*,*,#7665,.F.);
#10379=ORIENTED_EDGE('',*,*,#7544,.F.);
#10380=ORIENTED_EDGE('',*,*,#7543,.F.);
#10381=ORIENTED_EDGE('',*,*,#7667,.F.);
#10382=ORIENTED_EDGE('',*,*,#7550,.F.);
#10383=ORIENTED_EDGE('',*,*,#7546,.F.);
#10384=ORIENTED_EDGE('',*,*,#7634,.F.);
#10385=ORIENTED_EDGE('',*,*,#7674,.T.);
#10386=ORIENTED_EDGE('',*,*,#7539,.F.);
#10387=ORIENTED_EDGE('',*,*,#7552,.T.);
#10388=ORIENTED_EDGE('',*,*,#7533,.F.);
#10389=ORIENTED_EDGE('',*,*,#7554,.T.);
#10390=ORIENTED_EDGE('',*,*,#7637,.F.);
#10391=ORIENTED_EDGE('',*,*,#7675,.T.);
#10392=ORIENTED_EDGE('',*,*,#7511,.F.);
#10393=ORIENTED_EDGE('',*,*,#7524,.T.);
#10394=ORIENTED_EDGE('',*,*,#7505,.F.);
#10395=ORIENTED_EDGE('',*,*,#7526,.T.);
#10396=ORIENTED_EDGE('',*,*,#7641,.F.);
#10397=ORIENTED_EDGE('',*,*,#7644,.F.);
#10398=ORIENTED_EDGE('',*,*,#7646,.F.);
#10399=ORIENTED_EDGE('',*,*,#7650,.F.);
#10400=ORIENTED_EDGE('',*,*,#7652,.F.);
#10401=ORIENTED_EDGE('',*,*,#7655,.F.);
#10402=ORIENTED_EDGE('',*,*,#7657,.F.);
#10403=ORIENTED_EDGE('',*,*,#7659,.F.);
#10404=ORIENTED_EDGE('',*,*,#7660,.F.);
#10405=ORIENTED_EDGE('',*,*,#7421,.T.);
#10406=ORIENTED_EDGE('',*,*,#7410,.F.);
#10407=ORIENTED_EDGE('',*,*,#7424,.T.);
#10408=ORIENTED_EDGE('',*,*,#7427,.F.);
#10409=ORIENTED_EDGE('',*,*,#7563,.T.);
#10410=ORIENTED_EDGE('',*,*,#7405,.T.);
#10411=ORIENTED_EDGE('',*,*,#7390,.F.);
#10412=ORIENTED_EDGE('',*,*,#7439,.T.);
#10413=ORIENTED_EDGE('',*,*,#7397,.F.);
#10414=ORIENTED_EDGE('',*,*,#7402,.T.);
#10415=ORIENTED_EDGE('',*,*,#7472,.F.);
#10416=ORIENTED_EDGE('',*,*,#7501,.T.);
#10417=ORIENTED_EDGE('',*,*,#7477,.F.);
#10418=ORIENTED_EDGE('',*,*,#7371,.T.);
#10419=ORIENTED_EDGE('',*,*,#7381,.F.);
#10420=ORIENTED_EDGE('',*,*,#7383,.T.);
#10421=ORIENTED_EDGE('',*,*,#7376,.F.);
#10422=ORIENTED_EDGE('',*,*,#7374,.T.);
#10423=ORIENTED_EDGE('',*,*,#7359,.F.);
#10424=ORIENTED_EDGE('',*,*,#7433,.T.);
#10425=ORIENTED_EDGE('',*,*,#7366,.F.);
#10426=ORIENTED_EDGE('',*,*,#7512,.F.);
#10427=ORIENTED_EDGE('',*,*,#7675,.F.);
#10428=ORIENTED_EDGE('',*,*,#7638,.F.);
#10429=ORIENTED_EDGE('',*,*,#7516,.F.);
#10430=ORIENTED_EDGE('',*,*,#7515,.F.);
#10431=ORIENTED_EDGE('',*,*,#7663,.F.);
#10432=ORIENTED_EDGE('',*,*,#7522,.F.);
#10433=ORIENTED_EDGE('',*,*,#7518,.F.);
#10434=ORIENTED_EDGE('',*,*,#7676,.T.);
#10435=ORIENTED_EDGE('',*,*,#7631,.T.);
#10436=ORIENTED_EDGE('',*,*,#7677,.T.);
#10437=ORIENTED_EDGE('',*,*,#7678,.T.);
#10438=ORIENTED_EDGE('',*,*,#7679,.T.);
#10439=ORIENTED_EDGE('',*,*,#7680,.T.);
#10440=ORIENTED_EDGE('',*,*,#7681,.T.);
#10441=ORIENTED_EDGE('',*,*,#7682,.T.);
#10442=ORIENTED_EDGE('',*,*,#7599,.T.);
#10443=ORIENTED_EDGE('',*,*,#7679,.F.);
#10444=ORIENTED_EDGE('',*,*,#7632,.T.);
#10445=ORIENTED_EDGE('',*,*,#7676,.F.);
#10446=ORIENTED_EDGE('',*,*,#7683,.T.);
#10447=ORIENTED_EDGE('',*,*,#7677,.F.);
#10448=ORIENTED_EDGE('',*,*,#7630,.T.);
#10449=ORIENTED_EDGE('',*,*,#7682,.F.);
#10450=ORIENTED_EDGE('',*,*,#7684,.T.);
#10451=ORIENTED_EDGE('',*,*,#7680,.F.);
#10452=ORIENTED_EDGE('',*,*,#7683,.F.);
#10453=ORIENTED_EDGE('',*,*,#7678,.F.);
#10454=ORIENTED_EDGE('',*,*,#7684,.F.);
#10455=ORIENTED_EDGE('',*,*,#7681,.F.);
#10456=ORIENTED_EDGE('',*,*,#7685,.T.);
#10457=ORIENTED_EDGE('',*,*,#7686,.T.);
#10458=ORIENTED_EDGE('',*,*,#7685,.F.);
#10459=ORIENTED_EDGE('',*,*,#7687,.T.);
#10460=ORIENTED_EDGE('',*,*,#7672,.T.);
#10461=ORIENTED_EDGE('',*,*,#7688,.T.);
#10462=ORIENTED_EDGE('',*,*,#7689,.T.);
#10463=ORIENTED_EDGE('',*,*,#7690,.T.);
#10464=ORIENTED_EDGE('',*,*,#7691,.T.);
#10465=ORIENTED_EDGE('',*,*,#7692,.T.);
#10466=ORIENTED_EDGE('',*,*,#7693,.T.);
#10467=ORIENTED_EDGE('',*,*,#7586,.T.);
#10468=ORIENTED_EDGE('',*,*,#7691,.F.);
#10469=ORIENTED_EDGE('',*,*,#7673,.T.);
#10470=ORIENTED_EDGE('',*,*,#7687,.F.);
#10471=ORIENTED_EDGE('',*,*,#7694,.T.);
#10472=ORIENTED_EDGE('',*,*,#7688,.F.);
#10473=ORIENTED_EDGE('',*,*,#7671,.T.);
#10474=ORIENTED_EDGE('',*,*,#7693,.F.);
#10475=ORIENTED_EDGE('',*,*,#7695,.T.);
#10476=ORIENTED_EDGE('',*,*,#7692,.F.);
#10477=ORIENTED_EDGE('',*,*,#7694,.F.);
#10478=ORIENTED_EDGE('',*,*,#7690,.F.);
#10479=ORIENTED_EDGE('',*,*,#7696,.T.);
#10480=ORIENTED_EDGE('',*,*,#7697,.T.);
#10481=ORIENTED_EDGE('',*,*,#7696,.F.);
#10482=ORIENTED_EDGE('',*,*,#7689,.F.);
#10483=ORIENTED_EDGE('',*,*,#7695,.F.);
#10484=ORIENTED_EDGE('',*,*,#7629,.T.);
#10485=ORIENTED_EDGE('',*,*,#7698,.T.);
#10486=ORIENTED_EDGE('',*,*,#7699,.T.);
#10487=ORIENTED_EDGE('',*,*,#7698,.F.);
#10488=ORIENTED_EDGE('',*,*,#7699,.F.);
#10489=ORIENTED_EDGE('',*,*,#7700,.T.);
#10490=ORIENTED_EDGE('',*,*,#7701,.F.);
#10491=ORIENTED_EDGE('',*,*,#7700,.F.);
#10492=ORIENTED_EDGE('',*,*,#7702,.T.);
#10493=ORIENTED_EDGE('',*,*,#7703,.T.);
#10494=ORIENTED_EDGE('',*,*,#7701,.T.);
#10495=ORIENTED_EDGE('',*,*,#7703,.F.);
#10496=ORIENTED_EDGE('',*,*,#7580,.F.);
#10497=ORIENTED_EDGE('',*,*,#7576,.T.);
#10498=ORIENTED_EDGE('',*,*,#7704,.T.);
#10499=ORIENTED_EDGE('',*,*,#7705,.F.);
#10500=ORIENTED_EDGE('',*,*,#7702,.F.);
#10501=ORIENTED_EDGE('',*,*,#7697,.F.);
#10502=ORIENTED_EDGE('',*,*,#7686,.F.);
#10503=ORIENTED_EDGE('',*,*,#7490,.F.);
#10504=ORIENTED_EDGE('',*,*,#7706,.T.);
#10505=ORIENTED_EDGE('',*,*,#7468,.T.);
#10506=ORIENTED_EDGE('',*,*,#7500,.F.);
#10507=ORIENTED_EDGE('',*,*,#7495,.F.);
#10508=ORIENTED_EDGE('',*,*,#7707,.T.);
#10509=ORIENTED_EDGE('',*,*,#7469,.T.);
#10510=ORIENTED_EDGE('',*,*,#7706,.F.);
#10511=ORIENTED_EDGE('',*,*,#7481,.F.);
#10512=ORIENTED_EDGE('',*,*,#7498,.T.);
#10513=ORIENTED_EDGE('',*,*,#7470,.T.);
#10514=ORIENTED_EDGE('',*,*,#7707,.F.);
#10515=ORIENTED_EDGE('',*,*,#7456,.F.);
#10516=ORIENTED_EDGE('',*,*,#7708,.T.);
#10517=ORIENTED_EDGE('',*,*,#7444,.T.);
#10518=ORIENTED_EDGE('',*,*,#7463,.F.);
#10519=ORIENTED_EDGE('',*,*,#7459,.F.);
#10520=ORIENTED_EDGE('',*,*,#7709,.T.);
#10521=ORIENTED_EDGE('',*,*,#7445,.T.);
#10522=ORIENTED_EDGE('',*,*,#7708,.F.);
#10523=ORIENTED_EDGE('',*,*,#7449,.F.);
#10524=ORIENTED_EDGE('',*,*,#7461,.T.);
#10525=ORIENTED_EDGE('',*,*,#7446,.T.);
#10526=ORIENTED_EDGE('',*,*,#7709,.F.);
#10527=ORIENTED_EDGE('',*,*,#7582,.F.);
#10528=ORIENTED_EDGE('',*,*,#7705,.T.);
#10529=ORIENTED_EDGE('',*,*,#7710,.T.);
#10530=ORIENTED_EDGE('',*,*,#7577,.F.);
#10531=ORIENTED_EDGE('',*,*,#7710,.F.);
#10532=ORIENTED_EDGE('',*,*,#7704,.F.);
#10533=ORIENTED_EDGE('',*,*,#7575,.F.);
#10534=ORIENTED_EDGE('',*,*,#7578,.F.);
#10535=ORIENTED_EDGE('',*,*,#7414,.F.);
#10536=ORIENTED_EDGE('',*,*,#7664,.F.);
#10537=ORIENTED_EDGE('',*,*,#7558,.F.);
#10538=ORIENTED_EDGE('',*,*,#7419,.F.);
#10539=ORIENTED_EDGE('',*,*,#7711,.T.);
#10540=ORIENTED_EDGE('',*,*,#7712,.T.);
#10541=ORIENTED_EDGE('',*,*,#7713,.T.);
#10542=ORIENTED_EDGE('',*,*,#7712,.F.);
#10543=ORIENTED_EDGE('',*,*,#7714,.F.);
#10544=ORIENTED_EDGE('',*,*,#7715,.T.);
#10545=ORIENTED_EDGE('',*,*,#7713,.F.);
#10546=ORIENTED_EDGE('',*,*,#7715,.F.);
#10547=ORIENTED_EDGE('',*,*,#7716,.F.);
#10548=ORIENTED_EDGE('',*,*,#7717,.F.);
#10549=ORIENTED_EDGE('',*,*,#7718,.F.);
#10550=ORIENTED_EDGE('',*,*,#7719,.F.);
#10551=ORIENTED_EDGE('',*,*,#7720,.F.);
#10552=ORIENTED_EDGE('',*,*,#7721,.F.);
#10553=ORIENTED_EDGE('',*,*,#7722,.F.);
#10554=ORIENTED_EDGE('',*,*,#7723,.F.);
#10555=ORIENTED_EDGE('',*,*,#7724,.T.);
#10556=ORIENTED_EDGE('',*,*,#7725,.T.);
#10557=ORIENTED_EDGE('',*,*,#7711,.F.);
#10558=ORIENTED_EDGE('',*,*,#7726,.T.);
#10559=ORIENTED_EDGE('',*,*,#7727,.T.);
#10560=ORIENTED_EDGE('',*,*,#7714,.T.);
#10561=ORIENTED_EDGE('',*,*,#7727,.F.);
#10562=ORIENTED_EDGE('',*,*,#7728,.F.);
#10563=ORIENTED_EDGE('',*,*,#7729,.F.);
#10564=ORIENTED_EDGE('',*,*,#7730,.F.);
#10565=ORIENTED_EDGE('',*,*,#7731,.F.);
#10566=ORIENTED_EDGE('',*,*,#7732,.F.);
#10567=ORIENTED_EDGE('',*,*,#7733,.F.);
#10568=ORIENTED_EDGE('',*,*,#7734,.F.);
#10569=ORIENTED_EDGE('',*,*,#7735,.F.);
#10570=ORIENTED_EDGE('',*,*,#7736,.T.);
#10571=ORIENTED_EDGE('',*,*,#7737,.T.);
#10572=ORIENTED_EDGE('',*,*,#7726,.F.);
#10573=ORIENTED_EDGE('',*,*,#7738,.T.);
#10574=ORIENTED_EDGE('',*,*,#7716,.T.);
#10575=ORIENTED_EDGE('',*,*,#7739,.T.);
#10576=ORIENTED_EDGE('',*,*,#7740,.T.);
#10577=ORIENTED_EDGE('',*,*,#7738,.F.);
#10578=ORIENTED_EDGE('',*,*,#7741,.T.);
#10579=ORIENTED_EDGE('',*,*,#7742,.T.);
#10580=ORIENTED_EDGE('',*,*,#7717,.T.);
#10581=ORIENTED_EDGE('',*,*,#7743,.T.);
#10582=ORIENTED_EDGE('',*,*,#7718,.T.);
#10583=ORIENTED_EDGE('',*,*,#7742,.F.);
#10584=ORIENTED_EDGE('',*,*,#7744,.T.);
#10585=ORIENTED_EDGE('',*,*,#7743,.F.);
#10586=ORIENTED_EDGE('',*,*,#7745,.T.);
#10587=ORIENTED_EDGE('',*,*,#7746,.T.);
#10588=ORIENTED_EDGE('',*,*,#7719,.T.);
#10589=ORIENTED_EDGE('',*,*,#7747,.T.);
#10590=ORIENTED_EDGE('',*,*,#7720,.T.);
#10591=ORIENTED_EDGE('',*,*,#7746,.F.);
#10592=ORIENTED_EDGE('',*,*,#7748,.T.);
#10593=ORIENTED_EDGE('',*,*,#7747,.F.);
#10594=ORIENTED_EDGE('',*,*,#7749,.T.);
#10595=ORIENTED_EDGE('',*,*,#7750,.T.);
#10596=ORIENTED_EDGE('',*,*,#7721,.T.);
#10597=ORIENTED_EDGE('',*,*,#7751,.T.);
#10598=ORIENTED_EDGE('',*,*,#7722,.T.);
#10599=ORIENTED_EDGE('',*,*,#7750,.F.);
#10600=ORIENTED_EDGE('',*,*,#7752,.T.);
#10601=ORIENTED_EDGE('',*,*,#7751,.F.);
#10602=ORIENTED_EDGE('',*,*,#7753,.T.);
#10603=ORIENTED_EDGE('',*,*,#7739,.F.);
#10604=ORIENTED_EDGE('',*,*,#7723,.T.);
#10605=ORIENTED_EDGE('',*,*,#7745,.F.);
#10606=ORIENTED_EDGE('',*,*,#7754,.T.);
#10607=ORIENTED_EDGE('',*,*,#7755,.F.);
#10608=ORIENTED_EDGE('',*,*,#7756,.T.);
#10609=ORIENTED_EDGE('',*,*,#7744,.F.);
#10610=ORIENTED_EDGE('',*,*,#7757,.F.);
#10611=ORIENTED_EDGE('',*,*,#7758,.F.);
#10612=ORIENTED_EDGE('',*,*,#7754,.F.);
#10613=ORIENTED_EDGE('',*,*,#7741,.F.);
#10614=ORIENTED_EDGE('',*,*,#7759,.T.);
#10615=ORIENTED_EDGE('',*,*,#7760,.F.);
#10616=ORIENTED_EDGE('',*,*,#7757,.T.);
#10617=ORIENTED_EDGE('',*,*,#7740,.F.);
#10618=ORIENTED_EDGE('',*,*,#7761,.F.);
#10619=ORIENTED_EDGE('',*,*,#7762,.F.);
#10620=ORIENTED_EDGE('',*,*,#7759,.F.);
#10621=ORIENTED_EDGE('',*,*,#7763,.T.);
#10622=ORIENTED_EDGE('',*,*,#7764,.T.);
#10623=ORIENTED_EDGE('',*,*,#7765,.T.);
#10624=ORIENTED_EDGE('',*,*,#7766,.T.);
#10625=ORIENTED_EDGE('',*,*,#7767,.T.);
#10626=ORIENTED_EDGE('',*,*,#7768,.T.);
#10627=ORIENTED_EDGE('',*,*,#7763,.F.);
#10628=ORIENTED_EDGE('',*,*,#7755,.T.);
#10629=ORIENTED_EDGE('',*,*,#7769,.T.);
#10630=ORIENTED_EDGE('',*,*,#7770,.T.);
#10631=ORIENTED_EDGE('',*,*,#7767,.F.);
#10632=ORIENTED_EDGE('',*,*,#7758,.T.);
#10633=ORIENTED_EDGE('',*,*,#7771,.T.);
#10634=ORIENTED_EDGE('',*,*,#7772,.T.);
#10635=ORIENTED_EDGE('',*,*,#7769,.F.);
#10636=ORIENTED_EDGE('',*,*,#7760,.T.);
#10637=ORIENTED_EDGE('',*,*,#7773,.T.);
#10638=ORIENTED_EDGE('',*,*,#7774,.T.);
#10639=ORIENTED_EDGE('',*,*,#7771,.F.);
#10640=ORIENTED_EDGE('',*,*,#7762,.T.);
#10641=ORIENTED_EDGE('',*,*,#7775,.T.);
#10642=ORIENTED_EDGE('',*,*,#7776,.T.);
#10643=ORIENTED_EDGE('',*,*,#7773,.F.);
#10644=ORIENTED_EDGE('',*,*,#7777,.T.);
#10645=ORIENTED_EDGE('',*,*,#7778,.T.);
#10646=ORIENTED_EDGE('',*,*,#7779,.T.);
#10647=ORIENTED_EDGE('',*,*,#7775,.F.);
#10648=ORIENTED_EDGE('',*,*,#7780,.T.);
#10649=ORIENTED_EDGE('',*,*,#7765,.F.);
#10650=ORIENTED_EDGE('',*,*,#7781,.T.);
#10651=ORIENTED_EDGE('',*,*,#7778,.F.);
#10652=ORIENTED_EDGE('',*,*,#7782,.T.);
#10653=ORIENTED_EDGE('',*,*,#7776,.F.);
#10654=ORIENTED_EDGE('',*,*,#7783,.F.);
#10655=ORIENTED_EDGE('',*,*,#7784,.F.);
#10656=ORIENTED_EDGE('',*,*,#7785,.T.);
#10657=ORIENTED_EDGE('',*,*,#7779,.F.);
#10658=ORIENTED_EDGE('',*,*,#7786,.F.);
#10659=ORIENTED_EDGE('',*,*,#7787,.F.);
#10660=ORIENTED_EDGE('',*,*,#7783,.T.);
#10661=ORIENTED_EDGE('',*,*,#7781,.F.);
#10662=ORIENTED_EDGE('',*,*,#7788,.F.);
#10663=ORIENTED_EDGE('',*,*,#7789,.F.);
#10664=ORIENTED_EDGE('',*,*,#7786,.T.);
#10665=ORIENTED_EDGE('',*,*,#7764,.F.);
#10666=ORIENTED_EDGE('',*,*,#7790,.F.);
#10667=ORIENTED_EDGE('',*,*,#7791,.F.);
#10668=ORIENTED_EDGE('',*,*,#7788,.T.);
#10669=ORIENTED_EDGE('',*,*,#7748,.F.);
#10670=ORIENTED_EDGE('',*,*,#7756,.F.);
#10671=ORIENTED_EDGE('',*,*,#7766,.F.);
#10672=ORIENTED_EDGE('',*,*,#7792,.F.);
#10673=ORIENTED_EDGE('',*,*,#7793,.T.);
#10674=ORIENTED_EDGE('',*,*,#7791,.T.);
#10675=ORIENTED_EDGE('',*,*,#7794,.T.);
#10676=ORIENTED_EDGE('',*,*,#7728,.T.);
#10677=ORIENTED_EDGE('',*,*,#7795,.T.);
#10678=ORIENTED_EDGE('',*,*,#7789,.T.);
#10679=ORIENTED_EDGE('',*,*,#7793,.F.);
#10680=ORIENTED_EDGE('',*,*,#7735,.T.);
#10681=ORIENTED_EDGE('',*,*,#7796,.T.);
#10682=ORIENTED_EDGE('',*,*,#7787,.T.);
#10683=ORIENTED_EDGE('',*,*,#7795,.F.);
#10684=ORIENTED_EDGE('',*,*,#7734,.T.);
#10685=ORIENTED_EDGE('',*,*,#7797,.T.);
#10686=ORIENTED_EDGE('',*,*,#7784,.T.);
#10687=ORIENTED_EDGE('',*,*,#7796,.F.);
#10688=ORIENTED_EDGE('',*,*,#7733,.T.);
#10689=ORIENTED_EDGE('',*,*,#7798,.T.);
#10690=ORIENTED_EDGE('',*,*,#7799,.T.);
#10691=ORIENTED_EDGE('',*,*,#7797,.F.);
#10692=ORIENTED_EDGE('',*,*,#7732,.T.);
#10693=ORIENTED_EDGE('',*,*,#7800,.T.);
#10694=ORIENTED_EDGE('',*,*,#7801,.T.);
#10695=ORIENTED_EDGE('',*,*,#7798,.F.);
#10696=ORIENTED_EDGE('',*,*,#7731,.T.);
#10697=ORIENTED_EDGE('',*,*,#7802,.T.);
#10698=ORIENTED_EDGE('',*,*,#7803,.T.);
#10699=ORIENTED_EDGE('',*,*,#7800,.F.);
#10700=ORIENTED_EDGE('',*,*,#7730,.T.);
#10701=ORIENTED_EDGE('',*,*,#7794,.F.);
#10702=ORIENTED_EDGE('',*,*,#7804,.T.);
#10703=ORIENTED_EDGE('',*,*,#7802,.F.);
#10704=ORIENTED_EDGE('',*,*,#7729,.T.);
#10705=ORIENTED_EDGE('',*,*,#7772,.F.);
#10706=ORIENTED_EDGE('',*,*,#7805,.F.);
#10707=ORIENTED_EDGE('',*,*,#7801,.F.);
#10708=ORIENTED_EDGE('',*,*,#7806,.T.);
#10709=ORIENTED_EDGE('',*,*,#7770,.F.);
#10710=ORIENTED_EDGE('',*,*,#7806,.F.);
#10711=ORIENTED_EDGE('',*,*,#7803,.F.);
#10712=ORIENTED_EDGE('',*,*,#7807,.F.);
#10713=ORIENTED_EDGE('',*,*,#7768,.F.);
#10714=ORIENTED_EDGE('',*,*,#7807,.T.);
#10715=ORIENTED_EDGE('',*,*,#7804,.F.);
#10716=ORIENTED_EDGE('',*,*,#7790,.T.);
#10717=ORIENTED_EDGE('',*,*,#7774,.F.);
#10718=ORIENTED_EDGE('',*,*,#7785,.F.);
#10719=ORIENTED_EDGE('',*,*,#7799,.F.);
#10720=ORIENTED_EDGE('',*,*,#7805,.T.);
#10721=ORIENTED_EDGE('',*,*,#7737,.F.);
#10722=ORIENTED_EDGE('',*,*,#7808,.T.);
#10723=ORIENTED_EDGE('',*,*,#7724,.F.);
#10724=ORIENTED_EDGE('',*,*,#7808,.F.);
#10725=ORIENTED_EDGE('',*,*,#7736,.F.);
#10726=ORIENTED_EDGE('',*,*,#7809,.T.);
#10727=ORIENTED_EDGE('',*,*,#7725,.F.);
#10728=ORIENTED_EDGE('',*,*,#7809,.F.);
#10729=ORIENTED_EDGE('',*,*,#7753,.F.);
#10730=ORIENTED_EDGE('',*,*,#7810,.T.);
#10731=ORIENTED_EDGE('',*,*,#7777,.F.);
#10732=ORIENTED_EDGE('',*,*,#7761,.T.);
#10733=ORIENTED_EDGE('',*,*,#7749,.F.);
#10734=ORIENTED_EDGE('',*,*,#7792,.T.);
#10735=ORIENTED_EDGE('',*,*,#7782,.F.);
#10736=ORIENTED_EDGE('',*,*,#7811,.T.);
#10737=ORIENTED_EDGE('',*,*,#7752,.F.);
#10738=ORIENTED_EDGE('',*,*,#7811,.F.);
#10739=ORIENTED_EDGE('',*,*,#7780,.F.);
#10740=ORIENTED_EDGE('',*,*,#7810,.F.);
#10741=ORIENTED_EDGE('',*,*,#7812,.F.);
#10742=ORIENTED_EDGE('',*,*,#7813,.T.);
#10743=ORIENTED_EDGE('',*,*,#7814,.F.);
#10744=ORIENTED_EDGE('',*,*,#7815,.F.);
#10745=ORIENTED_EDGE('',*,*,#7816,.F.);
#10746=ORIENTED_EDGE('',*,*,#7815,.T.);
#10747=ORIENTED_EDGE('',*,*,#7817,.F.);
#10748=ORIENTED_EDGE('',*,*,#7818,.F.);
#10749=ORIENTED_EDGE('',*,*,#7819,.F.);
#10750=ORIENTED_EDGE('',*,*,#7818,.T.);
#10751=ORIENTED_EDGE('',*,*,#7820,.F.);
#10752=ORIENTED_EDGE('',*,*,#7821,.F.);
#10753=ORIENTED_EDGE('',*,*,#7822,.F.);
#10754=ORIENTED_EDGE('',*,*,#7821,.T.);
#10755=ORIENTED_EDGE('',*,*,#7823,.F.);
#10756=ORIENTED_EDGE('',*,*,#7813,.F.);
#10757=ORIENTED_EDGE('',*,*,#7823,.T.);
#10758=ORIENTED_EDGE('',*,*,#7820,.T.);
#10759=ORIENTED_EDGE('',*,*,#7817,.T.);
#10760=ORIENTED_EDGE('',*,*,#7814,.T.);
#10761=ORIENTED_EDGE('',*,*,#7824,.F.);
#10762=ORIENTED_EDGE('',*,*,#7825,.T.);
#10763=ORIENTED_EDGE('',*,*,#7826,.F.);
#10764=ORIENTED_EDGE('',*,*,#7827,.F.);
#10765=ORIENTED_EDGE('',*,*,#7828,.F.);
#10766=ORIENTED_EDGE('',*,*,#7827,.T.);
#10767=ORIENTED_EDGE('',*,*,#7829,.F.);
#10768=ORIENTED_EDGE('',*,*,#7830,.F.);
#10769=ORIENTED_EDGE('',*,*,#7831,.F.);
#10770=ORIENTED_EDGE('',*,*,#7830,.T.);
#10771=ORIENTED_EDGE('',*,*,#7832,.F.);
#10772=ORIENTED_EDGE('',*,*,#7833,.F.);
#10773=ORIENTED_EDGE('',*,*,#7834,.F.);
#10774=ORIENTED_EDGE('',*,*,#7833,.T.);
#10775=ORIENTED_EDGE('',*,*,#7835,.F.);
#10776=ORIENTED_EDGE('',*,*,#7825,.F.);
#10777=ORIENTED_EDGE('',*,*,#7835,.T.);
#10778=ORIENTED_EDGE('',*,*,#7832,.T.);
#10779=ORIENTED_EDGE('',*,*,#7829,.T.);
#10780=ORIENTED_EDGE('',*,*,#7826,.T.);
#10781=ORIENTED_EDGE('',*,*,#7836,.F.);
#10782=ORIENTED_EDGE('',*,*,#7837,.T.);
#10783=ORIENTED_EDGE('',*,*,#7838,.F.);
#10784=ORIENTED_EDGE('',*,*,#7839,.F.);
#10785=ORIENTED_EDGE('',*,*,#7840,.F.);
#10786=ORIENTED_EDGE('',*,*,#7839,.T.);
#10787=ORIENTED_EDGE('',*,*,#7841,.F.);
#10788=ORIENTED_EDGE('',*,*,#7842,.F.);
#10789=ORIENTED_EDGE('',*,*,#7843,.F.);
#10790=ORIENTED_EDGE('',*,*,#7842,.T.);
#10791=ORIENTED_EDGE('',*,*,#7844,.F.);
#10792=ORIENTED_EDGE('',*,*,#7845,.F.);
#10793=ORIENTED_EDGE('',*,*,#7846,.F.);
#10794=ORIENTED_EDGE('',*,*,#7845,.T.);
#10795=ORIENTED_EDGE('',*,*,#7847,.F.);
#10796=ORIENTED_EDGE('',*,*,#7837,.F.);
#10797=ORIENTED_EDGE('',*,*,#7847,.T.);
#10798=ORIENTED_EDGE('',*,*,#7844,.T.);
#10799=ORIENTED_EDGE('',*,*,#7841,.T.);
#10800=ORIENTED_EDGE('',*,*,#7838,.T.);
#10801=ORIENTED_EDGE('',*,*,#7848,.F.);
#10802=ORIENTED_EDGE('',*,*,#7849,.T.);
#10803=ORIENTED_EDGE('',*,*,#7850,.F.);
#10804=ORIENTED_EDGE('',*,*,#7851,.F.);
#10805=ORIENTED_EDGE('',*,*,#7852,.F.);
#10806=ORIENTED_EDGE('',*,*,#7851,.T.);
#10807=ORIENTED_EDGE('',*,*,#7853,.F.);
#10808=ORIENTED_EDGE('',*,*,#7854,.F.);
#10809=ORIENTED_EDGE('',*,*,#7855,.F.);
#10810=ORIENTED_EDGE('',*,*,#7854,.T.);
#10811=ORIENTED_EDGE('',*,*,#7856,.F.);
#10812=ORIENTED_EDGE('',*,*,#7857,.F.);
#10813=ORIENTED_EDGE('',*,*,#7858,.F.);
#10814=ORIENTED_EDGE('',*,*,#7857,.T.);
#10815=ORIENTED_EDGE('',*,*,#7859,.F.);
#10816=ORIENTED_EDGE('',*,*,#7849,.F.);
#10817=ORIENTED_EDGE('',*,*,#7859,.T.);
#10818=ORIENTED_EDGE('',*,*,#7856,.T.);
#10819=ORIENTED_EDGE('',*,*,#7853,.T.);
#10820=ORIENTED_EDGE('',*,*,#7850,.T.);
#10821=ORIENTED_EDGE('',*,*,#7812,.T.);
#10822=ORIENTED_EDGE('',*,*,#7816,.T.);
#10823=ORIENTED_EDGE('',*,*,#7819,.T.);
#10824=ORIENTED_EDGE('',*,*,#7822,.T.);
#10825=ORIENTED_EDGE('',*,*,#7824,.T.);
#10826=ORIENTED_EDGE('',*,*,#7828,.T.);
#10827=ORIENTED_EDGE('',*,*,#7831,.T.);
#10828=ORIENTED_EDGE('',*,*,#7834,.T.);
#10829=ORIENTED_EDGE('',*,*,#7836,.T.);
#10830=ORIENTED_EDGE('',*,*,#7840,.T.);
#10831=ORIENTED_EDGE('',*,*,#7843,.T.);
#10832=ORIENTED_EDGE('',*,*,#7846,.T.);
#10833=ORIENTED_EDGE('',*,*,#7858,.T.);
#10834=ORIENTED_EDGE('',*,*,#7848,.T.);
#10835=ORIENTED_EDGE('',*,*,#7852,.T.);
#10836=ORIENTED_EDGE('',*,*,#7855,.T.);
#10837=ORIENTED_EDGE('',*,*,#7860,.F.);
#10838=ORIENTED_EDGE('',*,*,#7861,.F.);
#10839=ORIENTED_EDGE('',*,*,#7862,.F.);
#10840=ORIENTED_EDGE('',*,*,#7863,.F.);
#10841=ORIENTED_EDGE('',*,*,#7864,.F.);
#10842=ORIENTED_EDGE('',*,*,#7865,.F.);
#10843=ORIENTED_EDGE('',*,*,#7866,.F.);
#10844=ORIENTED_EDGE('',*,*,#7867,.F.);
#10845=ORIENTED_EDGE('',*,*,#7868,.F.);
#10846=ORIENTED_EDGE('',*,*,#7869,.F.);
#10847=ORIENTED_EDGE('',*,*,#7870,.F.);
#10848=ORIENTED_EDGE('',*,*,#7871,.F.);
#10849=ORIENTED_EDGE('',*,*,#7872,.F.);
#10850=ORIENTED_EDGE('',*,*,#7873,.F.);
#10851=ORIENTED_EDGE('',*,*,#7874,.F.);
#10852=ORIENTED_EDGE('',*,*,#7875,.F.);
#10853=ORIENTED_EDGE('',*,*,#7876,.F.);
#10854=ORIENTED_EDGE('',*,*,#7877,.F.);
#10855=ORIENTED_EDGE('',*,*,#7878,.F.);
#10856=ORIENTED_EDGE('',*,*,#7879,.F.);
#10857=ORIENTED_EDGE('',*,*,#7880,.F.);
#10858=ORIENTED_EDGE('',*,*,#7868,.T.);
#10859=ORIENTED_EDGE('',*,*,#7881,.T.);
#10860=ORIENTED_EDGE('',*,*,#7879,.T.);
#10861=ORIENTED_EDGE('',*,*,#7882,.T.);
#10862=ORIENTED_EDGE('',*,*,#7883,.F.);
#10863=ORIENTED_EDGE('',*,*,#7884,.F.);
#10864=ORIENTED_EDGE('',*,*,#7885,.F.);
#10865=ORIENTED_EDGE('',*,*,#7884,.T.);
#10866=ORIENTED_EDGE('',*,*,#7886,.T.);
#10867=ORIENTED_EDGE('',*,*,#7873,.T.);
#10868=ORIENTED_EDGE('',*,*,#7887,.T.);
#10869=ORIENTED_EDGE('',*,*,#7876,.T.);
#10870=ORIENTED_EDGE('',*,*,#7888,.T.);
#10871=ORIENTED_EDGE('',*,*,#7885,.T.);
#10872=ORIENTED_EDGE('',*,*,#7889,.T.);
#10873=ORIENTED_EDGE('',*,*,#7880,.T.);
#10874=ORIENTED_EDGE('',*,*,#7890,.T.);
#10875=ORIENTED_EDGE('',*,*,#7883,.T.);
#10876=ORIENTED_EDGE('',*,*,#7891,.T.);
#10877=ORIENTED_EDGE('',*,*,#7870,.T.);
#10878=ORIENTED_EDGE('',*,*,#7892,.T.);
#10879=ORIENTED_EDGE('',*,*,#7878,.T.);
#10880=ORIENTED_EDGE('',*,*,#7893,.T.);
#10881=ORIENTED_EDGE('',*,*,#7863,.T.);
#10882=ORIENTED_EDGE('',*,*,#7894,.T.);
#10883=ORIENTED_EDGE('',*,*,#7877,.T.);
#10884=ORIENTED_EDGE('',*,*,#7895,.T.);
#10885=ORIENTED_EDGE('',*,*,#7875,.T.);
#10886=ORIENTED_EDGE('',*,*,#7896,.T.);
#10887=ORIENTED_EDGE('',*,*,#7871,.T.);
#10888=ORIENTED_EDGE('',*,*,#7897,.T.);
#10889=ORIENTED_EDGE('',*,*,#7874,.T.);
#10890=ORIENTED_EDGE('',*,*,#7898,.T.);
#10891=ORIENTED_EDGE('',*,*,#7867,.T.);
#10892=ORIENTED_EDGE('',*,*,#7899,.T.);
#10893=ORIENTED_EDGE('',*,*,#7864,.T.);
#10894=ORIENTED_EDGE('',*,*,#7900,.T.);
#10895=ORIENTED_EDGE('',*,*,#7872,.T.);
#10896=ORIENTED_EDGE('',*,*,#7901,.T.);
#10897=ORIENTED_EDGE('',*,*,#7869,.T.);
#10898=ORIENTED_EDGE('',*,*,#7902,.T.);
#10899=ORIENTED_EDGE('',*,*,#7862,.T.);
#10900=ORIENTED_EDGE('',*,*,#7903,.T.);
#10901=ORIENTED_EDGE('',*,*,#7861,.T.);
#10902=ORIENTED_EDGE('',*,*,#7904,.T.);
#10903=ORIENTED_EDGE('',*,*,#7866,.T.);
#10904=ORIENTED_EDGE('',*,*,#7905,.T.);
#10905=ORIENTED_EDGE('',*,*,#7860,.T.);
#10906=ORIENTED_EDGE('',*,*,#7906,.T.);
#10907=ORIENTED_EDGE('',*,*,#7865,.T.);
#10908=ORIENTED_EDGE('',*,*,#7907,.T.);
#10909=ORIENTED_EDGE('',*,*,#7882,.F.);
#10910=ORIENTED_EDGE('',*,*,#7892,.F.);
#10911=ORIENTED_EDGE('',*,*,#7903,.F.);
#10912=ORIENTED_EDGE('',*,*,#7905,.F.);
#10913=ORIENTED_EDGE('',*,*,#7887,.F.);
#10914=ORIENTED_EDGE('',*,*,#7900,.F.);
#10915=ORIENTED_EDGE('',*,*,#7895,.F.);
#10916=ORIENTED_EDGE('',*,*,#7889,.F.);
#10917=ORIENTED_EDGE('',*,*,#7886,.F.);
#10918=ORIENTED_EDGE('',*,*,#7890,.F.);
#10919=ORIENTED_EDGE('',*,*,#7881,.F.);
#10920=ORIENTED_EDGE('',*,*,#7898,.F.);
#10921=ORIENTED_EDGE('',*,*,#7908,.T.);
#10922=ORIENTED_EDGE('',*,*,#7888,.F.);
#10923=ORIENTED_EDGE('',*,*,#7897,.F.);
#10924=ORIENTED_EDGE('',*,*,#7893,.F.);
#10925=ORIENTED_EDGE('',*,*,#7891,.F.);
#10926=ORIENTED_EDGE('',*,*,#7894,.F.);
#10927=ORIENTED_EDGE('',*,*,#7906,.F.);
#10928=ORIENTED_EDGE('',*,*,#7902,.F.);
#10929=ORIENTED_EDGE('',*,*,#7896,.F.);
#10930=ORIENTED_EDGE('',*,*,#7909,.T.);
#10931=ORIENTED_EDGE('',*,*,#7899,.F.);
#10932=ORIENTED_EDGE('',*,*,#7904,.F.);
#10933=ORIENTED_EDGE('',*,*,#7907,.F.);
#10934=ORIENTED_EDGE('',*,*,#7901,.F.);
#10935=ORIENTED_EDGE('',*,*,#7909,.F.);
#10936=ORIENTED_EDGE('',*,*,#7910,.T.);
#10937=ORIENTED_EDGE('',*,*,#7908,.F.);
#10938=ORIENTED_EDGE('',*,*,#7910,.F.);
#10939=ORIENTED_EDGE('',*,*,#7911,.F.);
#10940=ORIENTED_EDGE('',*,*,#7912,.T.);
#10941=ORIENTED_EDGE('',*,*,#7913,.T.);
#10942=ORIENTED_EDGE('',*,*,#7914,.T.);
#10943=ORIENTED_EDGE('',*,*,#7915,.F.);
#10944=ORIENTED_EDGE('',*,*,#7916,.T.);
#10945=ORIENTED_EDGE('',*,*,#7911,.T.);
#10946=ORIENTED_EDGE('',*,*,#7917,.T.);
#10947=ORIENTED_EDGE('',*,*,#7918,.F.);
#10948=ORIENTED_EDGE('',*,*,#7919,.T.);
#10949=ORIENTED_EDGE('',*,*,#7915,.T.);
#10950=ORIENTED_EDGE('',*,*,#7920,.T.);
#10951=ORIENTED_EDGE('',*,*,#7921,.F.);
#10952=ORIENTED_EDGE('',*,*,#7922,.T.);
#10953=ORIENTED_EDGE('',*,*,#7918,.T.);
#10954=ORIENTED_EDGE('',*,*,#7923,.T.);
#10955=ORIENTED_EDGE('',*,*,#7924,.F.);
#10956=ORIENTED_EDGE('',*,*,#7925,.T.);
#10957=ORIENTED_EDGE('',*,*,#7921,.T.);
#10958=ORIENTED_EDGE('',*,*,#7926,.T.);
#10959=ORIENTED_EDGE('',*,*,#7927,.F.);
#10960=ORIENTED_EDGE('',*,*,#7928,.T.);
#10961=ORIENTED_EDGE('',*,*,#7924,.T.);
#10962=ORIENTED_EDGE('',*,*,#7929,.T.);
#10963=ORIENTED_EDGE('',*,*,#7930,.F.);
#10964=ORIENTED_EDGE('',*,*,#7931,.T.);
#10965=ORIENTED_EDGE('',*,*,#7927,.T.);
#10966=ORIENTED_EDGE('',*,*,#7932,.T.);
#10967=ORIENTED_EDGE('',*,*,#7933,.F.);
#10968=ORIENTED_EDGE('',*,*,#7934,.T.);
#10969=ORIENTED_EDGE('',*,*,#7930,.T.);
#10970=ORIENTED_EDGE('',*,*,#7935,.T.);
#10971=ORIENTED_EDGE('',*,*,#7936,.F.);
#10972=ORIENTED_EDGE('',*,*,#7937,.T.);
#10973=ORIENTED_EDGE('',*,*,#7933,.T.);
#10974=ORIENTED_EDGE('',*,*,#7938,.T.);
#10975=ORIENTED_EDGE('',*,*,#7939,.F.);
#10976=ORIENTED_EDGE('',*,*,#7940,.T.);
#10977=ORIENTED_EDGE('',*,*,#7936,.T.);
#10978=ORIENTED_EDGE('',*,*,#7941,.T.);
#10979=ORIENTED_EDGE('',*,*,#7942,.F.);
#10980=ORIENTED_EDGE('',*,*,#7943,.T.);
#10981=ORIENTED_EDGE('',*,*,#7939,.T.);
#10982=ORIENTED_EDGE('',*,*,#7944,.T.);
#10983=ORIENTED_EDGE('',*,*,#7945,.F.);
#10984=ORIENTED_EDGE('',*,*,#7946,.T.);
#10985=ORIENTED_EDGE('',*,*,#7942,.T.);
#10986=ORIENTED_EDGE('',*,*,#7947,.T.);
#10987=ORIENTED_EDGE('',*,*,#7948,.F.);
#10988=ORIENTED_EDGE('',*,*,#7949,.T.);
#10989=ORIENTED_EDGE('',*,*,#7945,.T.);
#10990=ORIENTED_EDGE('',*,*,#7950,.T.);
#10991=ORIENTED_EDGE('',*,*,#7951,.F.);
#10992=ORIENTED_EDGE('',*,*,#7952,.T.);
#10993=ORIENTED_EDGE('',*,*,#7948,.T.);
#10994=ORIENTED_EDGE('',*,*,#7953,.T.);
#10995=ORIENTED_EDGE('',*,*,#7954,.F.);
#10996=ORIENTED_EDGE('',*,*,#7955,.T.);
#10997=ORIENTED_EDGE('',*,*,#7951,.T.);
#10998=ORIENTED_EDGE('',*,*,#7956,.T.);
#10999=ORIENTED_EDGE('',*,*,#7957,.F.);
#11000=ORIENTED_EDGE('',*,*,#7958,.T.);
#11001=ORIENTED_EDGE('',*,*,#7954,.T.);
#11002=ORIENTED_EDGE('',*,*,#7959,.T.);
#11003=ORIENTED_EDGE('',*,*,#7960,.F.);
#11004=ORIENTED_EDGE('',*,*,#7961,.T.);
#11005=ORIENTED_EDGE('',*,*,#7957,.T.);
#11006=ORIENTED_EDGE('',*,*,#7962,.T.);
#11007=ORIENTED_EDGE('',*,*,#7963,.F.);
#11008=ORIENTED_EDGE('',*,*,#7964,.T.);
#11009=ORIENTED_EDGE('',*,*,#7960,.T.);
#11010=ORIENTED_EDGE('',*,*,#7965,.T.);
#11011=ORIENTED_EDGE('',*,*,#7966,.F.);
#11012=ORIENTED_EDGE('',*,*,#7967,.T.);
#11013=ORIENTED_EDGE('',*,*,#7963,.T.);
#11014=ORIENTED_EDGE('',*,*,#7968,.T.);
#11015=ORIENTED_EDGE('',*,*,#7969,.F.);
#11016=ORIENTED_EDGE('',*,*,#7970,.T.);
#11017=ORIENTED_EDGE('',*,*,#7966,.T.);
#11018=ORIENTED_EDGE('',*,*,#7971,.T.);
#11019=ORIENTED_EDGE('',*,*,#7972,.F.);
#11020=ORIENTED_EDGE('',*,*,#7973,.T.);
#11021=ORIENTED_EDGE('',*,*,#7969,.T.);
#11022=ORIENTED_EDGE('',*,*,#7974,.T.);
#11023=ORIENTED_EDGE('',*,*,#7975,.F.);
#11024=ORIENTED_EDGE('',*,*,#7976,.T.);
#11025=ORIENTED_EDGE('',*,*,#7972,.T.);
#11026=ORIENTED_EDGE('',*,*,#7977,.T.);
#11027=ORIENTED_EDGE('',*,*,#7978,.F.);
#11028=ORIENTED_EDGE('',*,*,#7979,.T.);
#11029=ORIENTED_EDGE('',*,*,#7975,.T.);
#11030=ORIENTED_EDGE('',*,*,#7980,.T.);
#11031=ORIENTED_EDGE('',*,*,#7981,.F.);
#11032=ORIENTED_EDGE('',*,*,#7982,.T.);
#11033=ORIENTED_EDGE('',*,*,#7978,.T.);
#11034=ORIENTED_EDGE('',*,*,#7983,.T.);
#11035=ORIENTED_EDGE('',*,*,#7984,.F.);
#11036=ORIENTED_EDGE('',*,*,#7985,.T.);
#11037=ORIENTED_EDGE('',*,*,#7981,.T.);
#11038=ORIENTED_EDGE('',*,*,#7986,.T.);
#11039=ORIENTED_EDGE('',*,*,#7987,.F.);
#11040=ORIENTED_EDGE('',*,*,#7988,.T.);
#11041=ORIENTED_EDGE('',*,*,#7984,.T.);
#11042=ORIENTED_EDGE('',*,*,#7989,.T.);
#11043=ORIENTED_EDGE('',*,*,#7990,.F.);
#11044=ORIENTED_EDGE('',*,*,#7991,.T.);
#11045=ORIENTED_EDGE('',*,*,#7987,.T.);
#11046=ORIENTED_EDGE('',*,*,#7992,.T.);
#11047=ORIENTED_EDGE('',*,*,#7993,.F.);
#11048=ORIENTED_EDGE('',*,*,#7994,.T.);
#11049=ORIENTED_EDGE('',*,*,#7990,.T.);
#11050=ORIENTED_EDGE('',*,*,#7995,.T.);
#11051=ORIENTED_EDGE('',*,*,#7996,.F.);
#11052=ORIENTED_EDGE('',*,*,#7997,.T.);
#11053=ORIENTED_EDGE('',*,*,#7998,.F.);
#11054=ORIENTED_EDGE('',*,*,#7999,.F.);
#11055=ORIENTED_EDGE('',*,*,#8000,.F.);
#11056=ORIENTED_EDGE('',*,*,#8001,.T.);
#11057=ORIENTED_EDGE('',*,*,#7996,.T.);
#11058=ORIENTED_EDGE('',*,*,#8002,.F.);
#11059=ORIENTED_EDGE('',*,*,#8003,.F.);
#11060=ORIENTED_EDGE('',*,*,#8004,.T.);
#11061=ORIENTED_EDGE('',*,*,#8000,.T.);
#11062=ORIENTED_EDGE('',*,*,#8005,.F.);
#11063=ORIENTED_EDGE('',*,*,#8006,.F.);
#11064=ORIENTED_EDGE('',*,*,#8007,.T.);
#11065=ORIENTED_EDGE('',*,*,#8003,.T.);
#11066=ORIENTED_EDGE('',*,*,#8008,.F.);
#11067=ORIENTED_EDGE('',*,*,#8009,.F.);
#11068=ORIENTED_EDGE('',*,*,#8010,.T.);
#11069=ORIENTED_EDGE('',*,*,#8006,.T.);
#11070=ORIENTED_EDGE('',*,*,#8011,.F.);
#11071=ORIENTED_EDGE('',*,*,#8012,.F.);
#11072=ORIENTED_EDGE('',*,*,#8013,.T.);
#11073=ORIENTED_EDGE('',*,*,#8009,.T.);
#11074=ORIENTED_EDGE('',*,*,#8014,.F.);
#11075=ORIENTED_EDGE('',*,*,#8015,.F.);
#11076=ORIENTED_EDGE('',*,*,#8016,.T.);
#11077=ORIENTED_EDGE('',*,*,#8012,.T.);
#11078=ORIENTED_EDGE('',*,*,#8017,.F.);
#11079=ORIENTED_EDGE('',*,*,#8018,.F.);
#11080=ORIENTED_EDGE('',*,*,#8019,.T.);
#11081=ORIENTED_EDGE('',*,*,#8015,.T.);
#11082=ORIENTED_EDGE('',*,*,#8020,.F.);
#11083=ORIENTED_EDGE('',*,*,#8021,.F.);
#11084=ORIENTED_EDGE('',*,*,#8022,.T.);
#11085=ORIENTED_EDGE('',*,*,#8018,.T.);
#11086=ORIENTED_EDGE('',*,*,#8023,.F.);
#11087=ORIENTED_EDGE('',*,*,#8024,.F.);
#11088=ORIENTED_EDGE('',*,*,#8025,.T.);
#11089=ORIENTED_EDGE('',*,*,#8021,.T.);
#11090=ORIENTED_EDGE('',*,*,#8026,.F.);
#11091=ORIENTED_EDGE('',*,*,#8027,.F.);
#11092=ORIENTED_EDGE('',*,*,#8028,.T.);
#11093=ORIENTED_EDGE('',*,*,#8024,.T.);
#11094=ORIENTED_EDGE('',*,*,#8029,.F.);
#11095=ORIENTED_EDGE('',*,*,#8030,.F.);
#11096=ORIENTED_EDGE('',*,*,#8031,.T.);
#11097=ORIENTED_EDGE('',*,*,#8027,.T.);
#11098=ORIENTED_EDGE('',*,*,#8032,.F.);
#11099=ORIENTED_EDGE('',*,*,#8033,.F.);
#11100=ORIENTED_EDGE('',*,*,#8034,.T.);
#11101=ORIENTED_EDGE('',*,*,#8030,.T.);
#11102=ORIENTED_EDGE('',*,*,#8035,.F.);
#11103=ORIENTED_EDGE('',*,*,#8036,.F.);
#11104=ORIENTED_EDGE('',*,*,#8037,.T.);
#11105=ORIENTED_EDGE('',*,*,#8033,.T.);
#11106=ORIENTED_EDGE('',*,*,#8038,.F.);
#11107=ORIENTED_EDGE('',*,*,#8039,.F.);
#11108=ORIENTED_EDGE('',*,*,#8040,.T.);
#11109=ORIENTED_EDGE('',*,*,#8036,.T.);
#11110=ORIENTED_EDGE('',*,*,#8041,.F.);
#11111=ORIENTED_EDGE('',*,*,#8042,.F.);
#11112=ORIENTED_EDGE('',*,*,#8043,.T.);
#11113=ORIENTED_EDGE('',*,*,#8039,.T.);
#11114=ORIENTED_EDGE('',*,*,#8044,.F.);
#11115=ORIENTED_EDGE('',*,*,#8045,.F.);
#11116=ORIENTED_EDGE('',*,*,#8046,.T.);
#11117=ORIENTED_EDGE('',*,*,#8042,.T.);
#11118=ORIENTED_EDGE('',*,*,#8047,.F.);
#11119=ORIENTED_EDGE('',*,*,#8048,.F.);
#11120=ORIENTED_EDGE('',*,*,#8049,.T.);
#11121=ORIENTED_EDGE('',*,*,#8045,.T.);
#11122=ORIENTED_EDGE('',*,*,#8050,.F.);
#11123=ORIENTED_EDGE('',*,*,#8051,.F.);
#11124=ORIENTED_EDGE('',*,*,#8052,.T.);
#11125=ORIENTED_EDGE('',*,*,#8048,.T.);
#11126=ORIENTED_EDGE('',*,*,#8053,.F.);
#11127=ORIENTED_EDGE('',*,*,#8054,.F.);
#11128=ORIENTED_EDGE('',*,*,#8055,.T.);
#11129=ORIENTED_EDGE('',*,*,#8051,.T.);
#11130=ORIENTED_EDGE('',*,*,#8056,.F.);
#11131=ORIENTED_EDGE('',*,*,#8057,.F.);
#11132=ORIENTED_EDGE('',*,*,#8058,.T.);
#11133=ORIENTED_EDGE('',*,*,#8054,.T.);
#11134=ORIENTED_EDGE('',*,*,#8059,.F.);
#11135=ORIENTED_EDGE('',*,*,#8060,.F.);
#11136=ORIENTED_EDGE('',*,*,#8061,.T.);
#11137=ORIENTED_EDGE('',*,*,#8057,.T.);
#11138=ORIENTED_EDGE('',*,*,#8062,.F.);
#11139=ORIENTED_EDGE('',*,*,#8063,.F.);
#11140=ORIENTED_EDGE('',*,*,#8064,.T.);
#11141=ORIENTED_EDGE('',*,*,#8060,.T.);
#11142=ORIENTED_EDGE('',*,*,#8065,.F.);
#11143=ORIENTED_EDGE('',*,*,#8066,.F.);
#11144=ORIENTED_EDGE('',*,*,#8067,.T.);
#11145=ORIENTED_EDGE('',*,*,#8063,.T.);
#11146=ORIENTED_EDGE('',*,*,#8068,.F.);
#11147=ORIENTED_EDGE('',*,*,#8069,.F.);
#11148=ORIENTED_EDGE('',*,*,#8070,.T.);
#11149=ORIENTED_EDGE('',*,*,#8066,.T.);
#11150=ORIENTED_EDGE('',*,*,#8071,.F.);
#11151=ORIENTED_EDGE('',*,*,#8072,.F.);
#11152=ORIENTED_EDGE('',*,*,#8073,.T.);
#11153=ORIENTED_EDGE('',*,*,#8069,.T.);
#11154=ORIENTED_EDGE('',*,*,#8074,.F.);
#11155=ORIENTED_EDGE('',*,*,#8075,.F.);
#11156=ORIENTED_EDGE('',*,*,#8076,.T.);
#11157=ORIENTED_EDGE('',*,*,#8072,.T.);
#11158=ORIENTED_EDGE('',*,*,#8077,.F.);
#11159=ORIENTED_EDGE('',*,*,#8078,.T.);
#11160=ORIENTED_EDGE('',*,*,#8079,.T.);
#11161=ORIENTED_EDGE('',*,*,#8080,.T.);
#11162=ORIENTED_EDGE('',*,*,#8079,.F.);
#11163=ORIENTED_EDGE('',*,*,#8081,.T.);
#11164=ORIENTED_EDGE('',*,*,#8082,.T.);
#11165=ORIENTED_EDGE('',*,*,#8083,.T.);
#11166=ORIENTED_EDGE('',*,*,#8084,.T.);
#11167=ORIENTED_EDGE('',*,*,#8085,.T.);
#11168=ORIENTED_EDGE('',*,*,#8086,.T.);
#11169=ORIENTED_EDGE('',*,*,#8087,.T.);
#11170=ORIENTED_EDGE('',*,*,#8088,.T.);
#11171=ORIENTED_EDGE('',*,*,#8089,.T.);
#11172=ORIENTED_EDGE('',*,*,#8090,.T.);
#11173=ORIENTED_EDGE('',*,*,#8091,.T.);
#11174=ORIENTED_EDGE('',*,*,#8092,.T.);
#11175=ORIENTED_EDGE('',*,*,#8093,.T.);
#11176=ORIENTED_EDGE('',*,*,#8094,.T.);
#11177=ORIENTED_EDGE('',*,*,#8095,.T.);
#11178=ORIENTED_EDGE('',*,*,#8096,.T.);
#11179=ORIENTED_EDGE('',*,*,#8097,.T.);
#11180=ORIENTED_EDGE('',*,*,#8098,.T.);
#11181=ORIENTED_EDGE('',*,*,#8099,.T.);
#11182=ORIENTED_EDGE('',*,*,#8100,.T.);
#11183=ORIENTED_EDGE('',*,*,#8101,.T.);
#11184=ORIENTED_EDGE('',*,*,#8102,.T.);
#11185=ORIENTED_EDGE('',*,*,#8103,.T.);
#11186=ORIENTED_EDGE('',*,*,#8104,.T.);
#11187=ORIENTED_EDGE('',*,*,#8105,.T.);
#11188=ORIENTED_EDGE('',*,*,#8106,.T.);
#11189=ORIENTED_EDGE('',*,*,#8107,.T.);
#11190=ORIENTED_EDGE('',*,*,#8108,.T.);
#11191=ORIENTED_EDGE('',*,*,#8109,.T.);
#11192=ORIENTED_EDGE('',*,*,#8110,.T.);
#11193=ORIENTED_EDGE('',*,*,#8111,.T.);
#11194=ORIENTED_EDGE('',*,*,#8112,.T.);
#11195=ORIENTED_EDGE('',*,*,#8113,.T.);
#11196=ORIENTED_EDGE('',*,*,#8114,.T.);
#11197=ORIENTED_EDGE('',*,*,#8115,.T.);
#11198=ORIENTED_EDGE('',*,*,#8116,.T.);
#11199=ORIENTED_EDGE('',*,*,#8117,.T.);
#11200=ORIENTED_EDGE('',*,*,#8118,.T.);
#11201=ORIENTED_EDGE('',*,*,#8119,.T.);
#11202=ORIENTED_EDGE('',*,*,#8120,.T.);
#11203=ORIENTED_EDGE('',*,*,#8121,.T.);
#11204=ORIENTED_EDGE('',*,*,#8122,.T.);
#11205=ORIENTED_EDGE('',*,*,#8123,.T.);
#11206=ORIENTED_EDGE('',*,*,#8124,.T.);
#11207=ORIENTED_EDGE('',*,*,#8125,.T.);
#11208=ORIENTED_EDGE('',*,*,#8126,.T.);
#11209=ORIENTED_EDGE('',*,*,#8127,.T.);
#11210=ORIENTED_EDGE('',*,*,#8128,.T.);
#11211=ORIENTED_EDGE('',*,*,#8129,.F.);
#11212=ORIENTED_EDGE('',*,*,#8130,.T.);
#11213=ORIENTED_EDGE('',*,*,#8131,.T.);
#11214=ORIENTED_EDGE('',*,*,#8132,.T.);
#11215=ORIENTED_EDGE('',*,*,#8104,.F.);
#11216=ORIENTED_EDGE('',*,*,#8133,.T.);
#11217=ORIENTED_EDGE('',*,*,#8134,.T.);
#11218=ORIENTED_EDGE('',*,*,#8135,.T.);
#11219=ORIENTED_EDGE('',*,*,#8102,.F.);
#11220=ORIENTED_EDGE('',*,*,#8136,.T.);
#11221=ORIENTED_EDGE('',*,*,#8137,.T.);
#11222=ORIENTED_EDGE('',*,*,#8138,.T.);
#11223=ORIENTED_EDGE('',*,*,#8100,.F.);
#11224=ORIENTED_EDGE('',*,*,#8139,.T.);
#11225=ORIENTED_EDGE('',*,*,#8140,.T.);
#11226=ORIENTED_EDGE('',*,*,#8141,.T.);
#11227=ORIENTED_EDGE('',*,*,#8098,.F.);
#11228=ORIENTED_EDGE('',*,*,#8142,.T.);
#11229=ORIENTED_EDGE('',*,*,#8143,.T.);
#11230=ORIENTED_EDGE('',*,*,#8144,.T.);
#11231=ORIENTED_EDGE('',*,*,#8096,.F.);
#11232=ORIENTED_EDGE('',*,*,#8145,.T.);
#11233=ORIENTED_EDGE('',*,*,#8146,.T.);
#11234=ORIENTED_EDGE('',*,*,#8147,.T.);
#11235=ORIENTED_EDGE('',*,*,#8094,.F.);
#11236=ORIENTED_EDGE('',*,*,#8148,.T.);
#11237=ORIENTED_EDGE('',*,*,#8149,.T.);
#11238=ORIENTED_EDGE('',*,*,#8150,.T.);
#11239=ORIENTED_EDGE('',*,*,#8092,.F.);
#11240=ORIENTED_EDGE('',*,*,#8151,.T.);
#11241=ORIENTED_EDGE('',*,*,#8152,.T.);
#11242=ORIENTED_EDGE('',*,*,#8153,.T.);
#11243=ORIENTED_EDGE('',*,*,#8090,.F.);
#11244=ORIENTED_EDGE('',*,*,#8154,.T.);
#11245=ORIENTED_EDGE('',*,*,#8155,.T.);
#11246=ORIENTED_EDGE('',*,*,#8156,.T.);
#11247=ORIENTED_EDGE('',*,*,#8088,.F.);
#11248=ORIENTED_EDGE('',*,*,#8157,.T.);
#11249=ORIENTED_EDGE('',*,*,#8158,.T.);
#11250=ORIENTED_EDGE('',*,*,#8159,.T.);
#11251=ORIENTED_EDGE('',*,*,#8086,.F.);
#11252=ORIENTED_EDGE('',*,*,#8160,.T.);
#11253=ORIENTED_EDGE('',*,*,#8161,.T.);
#11254=ORIENTED_EDGE('',*,*,#8162,.T.);
#11255=ORIENTED_EDGE('',*,*,#8084,.F.);
#11256=ORIENTED_EDGE('',*,*,#8163,.T.);
#11257=ORIENTED_EDGE('',*,*,#8164,.T.);
#11258=ORIENTED_EDGE('',*,*,#8165,.T.);
#11259=ORIENTED_EDGE('',*,*,#8082,.F.);
#11260=ORIENTED_EDGE('',*,*,#8166,.T.);
#11261=ORIENTED_EDGE('',*,*,#8167,.T.);
#11262=ORIENTED_EDGE('',*,*,#8168,.T.);
#11263=ORIENTED_EDGE('',*,*,#8128,.F.);
#11264=ORIENTED_EDGE('',*,*,#8169,.T.);
#11265=ORIENTED_EDGE('',*,*,#8170,.T.);
#11266=ORIENTED_EDGE('',*,*,#8171,.T.);
#11267=ORIENTED_EDGE('',*,*,#8126,.F.);
#11268=ORIENTED_EDGE('',*,*,#8172,.T.);
#11269=ORIENTED_EDGE('',*,*,#8173,.T.);
#11270=ORIENTED_EDGE('',*,*,#8174,.T.);
#11271=ORIENTED_EDGE('',*,*,#8124,.F.);
#11272=ORIENTED_EDGE('',*,*,#8175,.T.);
#11273=ORIENTED_EDGE('',*,*,#8176,.T.);
#11274=ORIENTED_EDGE('',*,*,#8177,.T.);
#11275=ORIENTED_EDGE('',*,*,#8122,.F.);
#11276=ORIENTED_EDGE('',*,*,#8178,.T.);
#11277=ORIENTED_EDGE('',*,*,#8179,.T.);
#11278=ORIENTED_EDGE('',*,*,#8180,.T.);
#11279=ORIENTED_EDGE('',*,*,#8120,.F.);
#11280=ORIENTED_EDGE('',*,*,#8181,.T.);
#11281=ORIENTED_EDGE('',*,*,#8182,.T.);
#11282=ORIENTED_EDGE('',*,*,#8183,.T.);
#11283=ORIENTED_EDGE('',*,*,#8118,.F.);
#11284=ORIENTED_EDGE('',*,*,#8184,.T.);
#11285=ORIENTED_EDGE('',*,*,#8185,.T.);
#11286=ORIENTED_EDGE('',*,*,#8186,.T.);
#11287=ORIENTED_EDGE('',*,*,#8116,.F.);
#11288=ORIENTED_EDGE('',*,*,#8187,.T.);
#11289=ORIENTED_EDGE('',*,*,#8188,.T.);
#11290=ORIENTED_EDGE('',*,*,#8189,.T.);
#11291=ORIENTED_EDGE('',*,*,#8114,.F.);
#11292=ORIENTED_EDGE('',*,*,#8190,.T.);
#11293=ORIENTED_EDGE('',*,*,#8191,.T.);
#11294=ORIENTED_EDGE('',*,*,#8192,.T.);
#11295=ORIENTED_EDGE('',*,*,#8112,.F.);
#11296=ORIENTED_EDGE('',*,*,#8193,.T.);
#11297=ORIENTED_EDGE('',*,*,#8194,.T.);
#11298=ORIENTED_EDGE('',*,*,#8195,.T.);
#11299=ORIENTED_EDGE('',*,*,#8110,.F.);
#11300=ORIENTED_EDGE('',*,*,#8196,.T.);
#11301=ORIENTED_EDGE('',*,*,#8197,.T.);
#11302=ORIENTED_EDGE('',*,*,#8198,.T.);
#11303=ORIENTED_EDGE('',*,*,#8108,.F.);
#11304=ORIENTED_EDGE('',*,*,#8199,.T.);
#11305=ORIENTED_EDGE('',*,*,#8200,.T.);
#11306=ORIENTED_EDGE('',*,*,#8201,.T.);
#11307=ORIENTED_EDGE('',*,*,#8106,.F.);
#11308=ORIENTED_EDGE('',*,*,#8202,.T.);
#11309=ORIENTED_EDGE('',*,*,#8203,.T.);
#11310=ORIENTED_EDGE('',*,*,#8130,.F.);
#11311=ORIENTED_EDGE('',*,*,#8080,.F.);
#11312=ORIENTED_EDGE('',*,*,#8204,.T.);
#11313=ORIENTED_EDGE('',*,*,#8205,.T.);
#11314=ORIENTED_EDGE('',*,*,#7998,.T.);
#11315=ORIENTED_EDGE('',*,*,#8206,.T.);
#11316=ORIENTED_EDGE('',*,*,#8205,.F.);
#11317=ORIENTED_EDGE('',*,*,#8207,.F.);
#11318=ORIENTED_EDGE('',*,*,#7995,.F.);
#11319=ORIENTED_EDGE('',*,*,#7992,.F.);
#11320=ORIENTED_EDGE('',*,*,#7989,.F.);
#11321=ORIENTED_EDGE('',*,*,#7986,.F.);
#11322=ORIENTED_EDGE('',*,*,#7983,.F.);
#11323=ORIENTED_EDGE('',*,*,#7980,.F.);
#11324=ORIENTED_EDGE('',*,*,#7977,.F.);
#11325=ORIENTED_EDGE('',*,*,#7974,.F.);
#11326=ORIENTED_EDGE('',*,*,#7971,.F.);
#11327=ORIENTED_EDGE('',*,*,#7968,.F.);
#11328=ORIENTED_EDGE('',*,*,#7965,.F.);
#11329=ORIENTED_EDGE('',*,*,#7962,.F.);
#11330=ORIENTED_EDGE('',*,*,#7959,.F.);
#11331=ORIENTED_EDGE('',*,*,#7956,.F.);
#11332=ORIENTED_EDGE('',*,*,#7953,.F.);
#11333=ORIENTED_EDGE('',*,*,#7950,.F.);
#11334=ORIENTED_EDGE('',*,*,#7947,.F.);
#11335=ORIENTED_EDGE('',*,*,#7944,.F.);
#11336=ORIENTED_EDGE('',*,*,#7941,.F.);
#11337=ORIENTED_EDGE('',*,*,#7938,.F.);
#11338=ORIENTED_EDGE('',*,*,#7935,.F.);
#11339=ORIENTED_EDGE('',*,*,#7932,.F.);
#11340=ORIENTED_EDGE('',*,*,#7929,.F.);
#11341=ORIENTED_EDGE('',*,*,#7926,.F.);
#11342=ORIENTED_EDGE('',*,*,#7923,.F.);
#11343=ORIENTED_EDGE('',*,*,#7920,.F.);
#11344=ORIENTED_EDGE('',*,*,#7917,.F.);
#11345=ORIENTED_EDGE('',*,*,#7914,.F.);
#11346=ORIENTED_EDGE('',*,*,#8208,.F.);
#11347=ORIENTED_EDGE('',*,*,#8209,.T.);
#11348=ORIENTED_EDGE('',*,*,#8077,.T.);
#11349=ORIENTED_EDGE('',*,*,#8074,.T.);
#11350=ORIENTED_EDGE('',*,*,#8071,.T.);
#11351=ORIENTED_EDGE('',*,*,#8068,.T.);
#11352=ORIENTED_EDGE('',*,*,#8065,.T.);
#11353=ORIENTED_EDGE('',*,*,#8062,.T.);
#11354=ORIENTED_EDGE('',*,*,#8059,.T.);
#11355=ORIENTED_EDGE('',*,*,#8056,.T.);
#11356=ORIENTED_EDGE('',*,*,#8053,.T.);
#11357=ORIENTED_EDGE('',*,*,#8050,.T.);
#11358=ORIENTED_EDGE('',*,*,#8047,.T.);
#11359=ORIENTED_EDGE('',*,*,#8044,.T.);
#11360=ORIENTED_EDGE('',*,*,#8041,.T.);
#11361=ORIENTED_EDGE('',*,*,#8038,.T.);
#11362=ORIENTED_EDGE('',*,*,#8035,.T.);
#11363=ORIENTED_EDGE('',*,*,#8032,.T.);
#11364=ORIENTED_EDGE('',*,*,#8029,.T.);
#11365=ORIENTED_EDGE('',*,*,#8026,.T.);
#11366=ORIENTED_EDGE('',*,*,#8023,.T.);
#11367=ORIENTED_EDGE('',*,*,#8020,.T.);
#11368=ORIENTED_EDGE('',*,*,#8017,.T.);
#11369=ORIENTED_EDGE('',*,*,#8014,.T.);
#11370=ORIENTED_EDGE('',*,*,#8011,.T.);
#11371=ORIENTED_EDGE('',*,*,#8008,.T.);
#11372=ORIENTED_EDGE('',*,*,#8005,.T.);
#11373=ORIENTED_EDGE('',*,*,#8002,.T.);
#11374=ORIENTED_EDGE('',*,*,#7999,.T.);
#11375=ORIENTED_EDGE('',*,*,#8210,.T.);
#11376=ORIENTED_EDGE('',*,*,#8211,.T.);
#11377=ORIENTED_EDGE('',*,*,#8212,.T.);
#11378=ORIENTED_EDGE('',*,*,#8213,.T.);
#11379=ORIENTED_EDGE('',*,*,#8208,.T.);
#11380=ORIENTED_EDGE('',*,*,#8075,.T.);
#11381=ORIENTED_EDGE('',*,*,#8209,.F.);
#11382=ORIENTED_EDGE('',*,*,#8213,.F.);
#11383=ORIENTED_EDGE('',*,*,#8214,.T.);
#11384=ORIENTED_EDGE('',*,*,#8206,.F.);
#11385=ORIENTED_EDGE('',*,*,#7997,.F.);
#11386=ORIENTED_EDGE('',*,*,#8001,.F.);
#11387=ORIENTED_EDGE('',*,*,#8004,.F.);
#11388=ORIENTED_EDGE('',*,*,#8007,.F.);
#11389=ORIENTED_EDGE('',*,*,#8010,.F.);
#11390=ORIENTED_EDGE('',*,*,#8013,.F.);
#11391=ORIENTED_EDGE('',*,*,#8016,.F.);
#11392=ORIENTED_EDGE('',*,*,#8019,.F.);
#11393=ORIENTED_EDGE('',*,*,#8022,.F.);
#11394=ORIENTED_EDGE('',*,*,#8025,.F.);
#11395=ORIENTED_EDGE('',*,*,#8028,.F.);
#11396=ORIENTED_EDGE('',*,*,#8031,.F.);
#11397=ORIENTED_EDGE('',*,*,#8034,.F.);
#11398=ORIENTED_EDGE('',*,*,#8037,.F.);
#11399=ORIENTED_EDGE('',*,*,#8040,.F.);
#11400=ORIENTED_EDGE('',*,*,#8043,.F.);
#11401=ORIENTED_EDGE('',*,*,#8046,.F.);
#11402=ORIENTED_EDGE('',*,*,#8049,.F.);
#11403=ORIENTED_EDGE('',*,*,#8052,.F.);
#11404=ORIENTED_EDGE('',*,*,#8055,.F.);
#11405=ORIENTED_EDGE('',*,*,#8058,.F.);
#11406=ORIENTED_EDGE('',*,*,#8061,.F.);
#11407=ORIENTED_EDGE('',*,*,#8064,.F.);
#11408=ORIENTED_EDGE('',*,*,#8067,.F.);
#11409=ORIENTED_EDGE('',*,*,#8070,.F.);
#11410=ORIENTED_EDGE('',*,*,#8073,.F.);
#11411=ORIENTED_EDGE('',*,*,#8076,.F.);
#11412=ORIENTED_EDGE('',*,*,#8214,.F.);
#11413=ORIENTED_EDGE('',*,*,#8212,.F.);
#11414=ORIENTED_EDGE('',*,*,#7912,.F.);
#11415=ORIENTED_EDGE('',*,*,#7916,.F.);
#11416=ORIENTED_EDGE('',*,*,#7919,.F.);
#11417=ORIENTED_EDGE('',*,*,#7922,.F.);
#11418=ORIENTED_EDGE('',*,*,#7925,.F.);
#11419=ORIENTED_EDGE('',*,*,#7928,.F.);
#11420=ORIENTED_EDGE('',*,*,#7931,.F.);
#11421=ORIENTED_EDGE('',*,*,#7934,.F.);
#11422=ORIENTED_EDGE('',*,*,#7937,.F.);
#11423=ORIENTED_EDGE('',*,*,#7940,.F.);
#11424=ORIENTED_EDGE('',*,*,#7943,.F.);
#11425=ORIENTED_EDGE('',*,*,#7946,.F.);
#11426=ORIENTED_EDGE('',*,*,#7949,.F.);
#11427=ORIENTED_EDGE('',*,*,#7952,.F.);
#11428=ORIENTED_EDGE('',*,*,#7955,.F.);
#11429=ORIENTED_EDGE('',*,*,#7958,.F.);
#11430=ORIENTED_EDGE('',*,*,#7961,.F.);
#11431=ORIENTED_EDGE('',*,*,#7964,.F.);
#11432=ORIENTED_EDGE('',*,*,#7967,.F.);
#11433=ORIENTED_EDGE('',*,*,#7970,.F.);
#11434=ORIENTED_EDGE('',*,*,#7973,.F.);
#11435=ORIENTED_EDGE('',*,*,#7976,.F.);
#11436=ORIENTED_EDGE('',*,*,#7979,.F.);
#11437=ORIENTED_EDGE('',*,*,#7982,.F.);
#11438=ORIENTED_EDGE('',*,*,#7985,.F.);
#11439=ORIENTED_EDGE('',*,*,#7988,.F.);
#11440=ORIENTED_EDGE('',*,*,#7991,.F.);
#11441=ORIENTED_EDGE('',*,*,#7994,.F.);
#11442=ORIENTED_EDGE('',*,*,#8215,.F.);
#11443=ORIENTED_EDGE('',*,*,#8165,.F.);
#11444=ORIENTED_EDGE('',*,*,#8216,.T.);
#11445=ORIENTED_EDGE('',*,*,#8217,.F.);
#11446=ORIENTED_EDGE('',*,*,#8218,.F.);
#11447=ORIENTED_EDGE('',*,*,#8083,.F.);
#11448=ORIENTED_EDGE('',*,*,#8218,.T.);
#11449=ORIENTED_EDGE('',*,*,#8219,.T.);
#11450=ORIENTED_EDGE('',*,*,#8163,.F.);
#11451=ORIENTED_EDGE('',*,*,#8219,.F.);
#11452=ORIENTED_EDGE('',*,*,#8217,.T.);
#11453=ORIENTED_EDGE('',*,*,#8220,.T.);
#11454=ORIENTED_EDGE('',*,*,#8164,.F.);
#11455=ORIENTED_EDGE('',*,*,#8220,.F.);
#11456=ORIENTED_EDGE('',*,*,#8216,.F.);
#11457=ORIENTED_EDGE('',*,*,#8162,.F.);
#11458=ORIENTED_EDGE('',*,*,#8221,.T.);
#11459=ORIENTED_EDGE('',*,*,#8222,.F.);
#11460=ORIENTED_EDGE('',*,*,#8223,.F.);
#11461=ORIENTED_EDGE('',*,*,#8085,.F.);
#11462=ORIENTED_EDGE('',*,*,#8223,.T.);
#11463=ORIENTED_EDGE('',*,*,#8224,.T.);
#11464=ORIENTED_EDGE('',*,*,#8160,.F.);
#11465=ORIENTED_EDGE('',*,*,#8224,.F.);
#11466=ORIENTED_EDGE('',*,*,#8222,.T.);
#11467=ORIENTED_EDGE('',*,*,#8225,.T.);
#11468=ORIENTED_EDGE('',*,*,#8161,.F.);
#11469=ORIENTED_EDGE('',*,*,#8225,.F.);
#11470=ORIENTED_EDGE('',*,*,#8221,.F.);
#11471=ORIENTED_EDGE('',*,*,#8159,.F.);
#11472=ORIENTED_EDGE('',*,*,#8226,.T.);
#11473=ORIENTED_EDGE('',*,*,#8227,.F.);
#11474=ORIENTED_EDGE('',*,*,#8228,.F.);
#11475=ORIENTED_EDGE('',*,*,#8087,.F.);
#11476=ORIENTED_EDGE('',*,*,#8228,.T.);
#11477=ORIENTED_EDGE('',*,*,#8229,.T.);
#11478=ORIENTED_EDGE('',*,*,#8157,.F.);
#11479=ORIENTED_EDGE('',*,*,#8229,.F.);
#11480=ORIENTED_EDGE('',*,*,#8227,.T.);
#11481=ORIENTED_EDGE('',*,*,#8230,.T.);
#11482=ORIENTED_EDGE('',*,*,#8158,.F.);
#11483=ORIENTED_EDGE('',*,*,#8230,.F.);
#11484=ORIENTED_EDGE('',*,*,#8226,.F.);
#11485=ORIENTED_EDGE('',*,*,#8156,.F.);
#11486=ORIENTED_EDGE('',*,*,#8231,.T.);
#11487=ORIENTED_EDGE('',*,*,#8232,.F.);
#11488=ORIENTED_EDGE('',*,*,#8233,.F.);
#11489=ORIENTED_EDGE('',*,*,#8089,.F.);
#11490=ORIENTED_EDGE('',*,*,#8233,.T.);
#11491=ORIENTED_EDGE('',*,*,#8234,.T.);
#11492=ORIENTED_EDGE('',*,*,#8154,.F.);
#11493=ORIENTED_EDGE('',*,*,#8234,.F.);
#11494=ORIENTED_EDGE('',*,*,#8232,.T.);
#11495=ORIENTED_EDGE('',*,*,#8235,.T.);
#11496=ORIENTED_EDGE('',*,*,#8155,.F.);
#11497=ORIENTED_EDGE('',*,*,#8235,.F.);
#11498=ORIENTED_EDGE('',*,*,#8231,.F.);
#11499=ORIENTED_EDGE('',*,*,#8153,.F.);
#11500=ORIENTED_EDGE('',*,*,#8236,.T.);
#11501=ORIENTED_EDGE('',*,*,#8237,.F.);
#11502=ORIENTED_EDGE('',*,*,#8238,.F.);
#11503=ORIENTED_EDGE('',*,*,#8091,.F.);
#11504=ORIENTED_EDGE('',*,*,#8238,.T.);
#11505=ORIENTED_EDGE('',*,*,#8239,.T.);
#11506=ORIENTED_EDGE('',*,*,#8151,.F.);
#11507=ORIENTED_EDGE('',*,*,#8239,.F.);
#11508=ORIENTED_EDGE('',*,*,#8237,.T.);
#11509=ORIENTED_EDGE('',*,*,#8240,.T.);
#11510=ORIENTED_EDGE('',*,*,#8152,.F.);
#11511=ORIENTED_EDGE('',*,*,#8240,.F.);
#11512=ORIENTED_EDGE('',*,*,#8236,.F.);
#11513=ORIENTED_EDGE('',*,*,#8150,.F.);
#11514=ORIENTED_EDGE('',*,*,#8241,.T.);
#11515=ORIENTED_EDGE('',*,*,#8242,.F.);
#11516=ORIENTED_EDGE('',*,*,#8243,.F.);
#11517=ORIENTED_EDGE('',*,*,#8093,.F.);
#11518=ORIENTED_EDGE('',*,*,#8243,.T.);
#11519=ORIENTED_EDGE('',*,*,#8244,.T.);
#11520=ORIENTED_EDGE('',*,*,#8148,.F.);
#11521=ORIENTED_EDGE('',*,*,#8244,.F.);
#11522=ORIENTED_EDGE('',*,*,#8242,.T.);
#11523=ORIENTED_EDGE('',*,*,#8245,.T.);
#11524=ORIENTED_EDGE('',*,*,#8149,.F.);
#11525=ORIENTED_EDGE('',*,*,#8245,.F.);
#11526=ORIENTED_EDGE('',*,*,#8241,.F.);
#11527=ORIENTED_EDGE('',*,*,#8147,.F.);
#11528=ORIENTED_EDGE('',*,*,#8246,.T.);
#11529=ORIENTED_EDGE('',*,*,#8247,.F.);
#11530=ORIENTED_EDGE('',*,*,#8248,.F.);
#11531=ORIENTED_EDGE('',*,*,#8095,.F.);
#11532=ORIENTED_EDGE('',*,*,#8248,.T.);
#11533=ORIENTED_EDGE('',*,*,#8249,.T.);
#11534=ORIENTED_EDGE('',*,*,#8145,.F.);
#11535=ORIENTED_EDGE('',*,*,#8249,.F.);
#11536=ORIENTED_EDGE('',*,*,#8247,.T.);
#11537=ORIENTED_EDGE('',*,*,#8250,.T.);
#11538=ORIENTED_EDGE('',*,*,#8146,.F.);
#11539=ORIENTED_EDGE('',*,*,#8250,.F.);
#11540=ORIENTED_EDGE('',*,*,#8246,.F.);
#11541=ORIENTED_EDGE('',*,*,#8144,.F.);
#11542=ORIENTED_EDGE('',*,*,#8251,.T.);
#11543=ORIENTED_EDGE('',*,*,#8252,.F.);
#11544=ORIENTED_EDGE('',*,*,#8253,.F.);
#11545=ORIENTED_EDGE('',*,*,#8097,.F.);
#11546=ORIENTED_EDGE('',*,*,#8253,.T.);
#11547=ORIENTED_EDGE('',*,*,#8254,.T.);
#11548=ORIENTED_EDGE('',*,*,#8142,.F.);
#11549=ORIENTED_EDGE('',*,*,#8254,.F.);
#11550=ORIENTED_EDGE('',*,*,#8252,.T.);
#11551=ORIENTED_EDGE('',*,*,#8255,.T.);
#11552=ORIENTED_EDGE('',*,*,#8143,.F.);
#11553=ORIENTED_EDGE('',*,*,#8255,.F.);
#11554=ORIENTED_EDGE('',*,*,#8251,.F.);
#11555=ORIENTED_EDGE('',*,*,#8141,.F.);
#11556=ORIENTED_EDGE('',*,*,#8256,.T.);
#11557=ORIENTED_EDGE('',*,*,#8257,.F.);
#11558=ORIENTED_EDGE('',*,*,#8258,.F.);
#11559=ORIENTED_EDGE('',*,*,#8099,.F.);
#11560=ORIENTED_EDGE('',*,*,#8258,.T.);
#11561=ORIENTED_EDGE('',*,*,#8259,.T.);
#11562=ORIENTED_EDGE('',*,*,#8139,.F.);
#11563=ORIENTED_EDGE('',*,*,#8259,.F.);
#11564=ORIENTED_EDGE('',*,*,#8257,.T.);
#11565=ORIENTED_EDGE('',*,*,#8260,.T.);
#11566=ORIENTED_EDGE('',*,*,#8140,.F.);
#11567=ORIENTED_EDGE('',*,*,#8260,.F.);
#11568=ORIENTED_EDGE('',*,*,#8256,.F.);
#11569=ORIENTED_EDGE('',*,*,#8138,.F.);
#11570=ORIENTED_EDGE('',*,*,#8261,.T.);
#11571=ORIENTED_EDGE('',*,*,#8262,.F.);
#11572=ORIENTED_EDGE('',*,*,#8263,.F.);
#11573=ORIENTED_EDGE('',*,*,#8101,.F.);
#11574=ORIENTED_EDGE('',*,*,#8263,.T.);
#11575=ORIENTED_EDGE('',*,*,#8264,.T.);
#11576=ORIENTED_EDGE('',*,*,#8136,.F.);
#11577=ORIENTED_EDGE('',*,*,#8264,.F.);
#11578=ORIENTED_EDGE('',*,*,#8262,.T.);
#11579=ORIENTED_EDGE('',*,*,#8265,.T.);
#11580=ORIENTED_EDGE('',*,*,#8137,.F.);
#11581=ORIENTED_EDGE('',*,*,#8265,.F.);
#11582=ORIENTED_EDGE('',*,*,#8261,.F.);
#11583=ORIENTED_EDGE('',*,*,#8135,.F.);
#11584=ORIENTED_EDGE('',*,*,#8266,.T.);
#11585=ORIENTED_EDGE('',*,*,#8267,.F.);
#11586=ORIENTED_EDGE('',*,*,#8268,.F.);
#11587=ORIENTED_EDGE('',*,*,#8103,.F.);
#11588=ORIENTED_EDGE('',*,*,#8268,.T.);
#11589=ORIENTED_EDGE('',*,*,#8269,.T.);
#11590=ORIENTED_EDGE('',*,*,#8133,.F.);
#11591=ORIENTED_EDGE('',*,*,#8269,.F.);
#11592=ORIENTED_EDGE('',*,*,#8267,.T.);
#11593=ORIENTED_EDGE('',*,*,#8270,.T.);
#11594=ORIENTED_EDGE('',*,*,#8134,.F.);
#11595=ORIENTED_EDGE('',*,*,#8270,.F.);
#11596=ORIENTED_EDGE('',*,*,#8266,.F.);
#11597=ORIENTED_EDGE('',*,*,#8132,.F.);
#11598=ORIENTED_EDGE('',*,*,#8271,.T.);
#11599=ORIENTED_EDGE('',*,*,#8272,.F.);
#11600=ORIENTED_EDGE('',*,*,#8273,.F.);
#11601=ORIENTED_EDGE('',*,*,#8105,.F.);
#11602=ORIENTED_EDGE('',*,*,#8273,.T.);
#11603=ORIENTED_EDGE('',*,*,#8274,.T.);
#11604=ORIENTED_EDGE('',*,*,#8202,.F.);
#11605=ORIENTED_EDGE('',*,*,#8274,.F.);
#11606=ORIENTED_EDGE('',*,*,#8272,.T.);
#11607=ORIENTED_EDGE('',*,*,#8275,.T.);
#11608=ORIENTED_EDGE('',*,*,#8203,.F.);
#11609=ORIENTED_EDGE('',*,*,#8275,.F.);
#11610=ORIENTED_EDGE('',*,*,#8271,.F.);
#11611=ORIENTED_EDGE('',*,*,#8131,.F.);
#11612=ORIENTED_EDGE('',*,*,#8201,.F.);
#11613=ORIENTED_EDGE('',*,*,#8276,.T.);
#11614=ORIENTED_EDGE('',*,*,#8277,.F.);
#11615=ORIENTED_EDGE('',*,*,#8278,.F.);
#11616=ORIENTED_EDGE('',*,*,#8107,.F.);
#11617=ORIENTED_EDGE('',*,*,#8278,.T.);
#11618=ORIENTED_EDGE('',*,*,#8279,.T.);
#11619=ORIENTED_EDGE('',*,*,#8199,.F.);
#11620=ORIENTED_EDGE('',*,*,#8279,.F.);
#11621=ORIENTED_EDGE('',*,*,#8277,.T.);
#11622=ORIENTED_EDGE('',*,*,#8280,.T.);
#11623=ORIENTED_EDGE('',*,*,#8200,.F.);
#11624=ORIENTED_EDGE('',*,*,#8280,.F.);
#11625=ORIENTED_EDGE('',*,*,#8276,.F.);
#11626=ORIENTED_EDGE('',*,*,#8198,.F.);
#11627=ORIENTED_EDGE('',*,*,#8281,.T.);
#11628=ORIENTED_EDGE('',*,*,#8282,.F.);
#11629=ORIENTED_EDGE('',*,*,#8283,.F.);
#11630=ORIENTED_EDGE('',*,*,#8109,.F.);
#11631=ORIENTED_EDGE('',*,*,#8283,.T.);
#11632=ORIENTED_EDGE('',*,*,#8284,.T.);
#11633=ORIENTED_EDGE('',*,*,#8196,.F.);
#11634=ORIENTED_EDGE('',*,*,#8284,.F.);
#11635=ORIENTED_EDGE('',*,*,#8282,.T.);
#11636=ORIENTED_EDGE('',*,*,#8285,.T.);
#11637=ORIENTED_EDGE('',*,*,#8197,.F.);
#11638=ORIENTED_EDGE('',*,*,#8285,.F.);
#11639=ORIENTED_EDGE('',*,*,#8281,.F.);
#11640=ORIENTED_EDGE('',*,*,#8195,.F.);
#11641=ORIENTED_EDGE('',*,*,#8286,.T.);
#11642=ORIENTED_EDGE('',*,*,#8287,.F.);
#11643=ORIENTED_EDGE('',*,*,#8288,.F.);
#11644=ORIENTED_EDGE('',*,*,#8111,.F.);
#11645=ORIENTED_EDGE('',*,*,#8288,.T.);
#11646=ORIENTED_EDGE('',*,*,#8289,.T.);
#11647=ORIENTED_EDGE('',*,*,#8193,.F.);
#11648=ORIENTED_EDGE('',*,*,#8289,.F.);
#11649=ORIENTED_EDGE('',*,*,#8287,.T.);
#11650=ORIENTED_EDGE('',*,*,#8290,.T.);
#11651=ORIENTED_EDGE('',*,*,#8194,.F.);
#11652=ORIENTED_EDGE('',*,*,#8290,.F.);
#11653=ORIENTED_EDGE('',*,*,#8286,.F.);
#11654=ORIENTED_EDGE('',*,*,#8192,.F.);
#11655=ORIENTED_EDGE('',*,*,#8291,.T.);
#11656=ORIENTED_EDGE('',*,*,#8292,.F.);
#11657=ORIENTED_EDGE('',*,*,#8293,.F.);
#11658=ORIENTED_EDGE('',*,*,#8113,.F.);
#11659=ORIENTED_EDGE('',*,*,#8293,.T.);
#11660=ORIENTED_EDGE('',*,*,#8294,.T.);
#11661=ORIENTED_EDGE('',*,*,#8190,.F.);
#11662=ORIENTED_EDGE('',*,*,#8294,.F.);
#11663=ORIENTED_EDGE('',*,*,#8292,.T.);
#11664=ORIENTED_EDGE('',*,*,#8295,.T.);
#11665=ORIENTED_EDGE('',*,*,#8191,.F.);
#11666=ORIENTED_EDGE('',*,*,#8295,.F.);
#11667=ORIENTED_EDGE('',*,*,#8291,.F.);
#11668=ORIENTED_EDGE('',*,*,#8189,.F.);
#11669=ORIENTED_EDGE('',*,*,#8296,.T.);
#11670=ORIENTED_EDGE('',*,*,#8297,.F.);
#11671=ORIENTED_EDGE('',*,*,#8298,.F.);
#11672=ORIENTED_EDGE('',*,*,#8115,.F.);
#11673=ORIENTED_EDGE('',*,*,#8298,.T.);
#11674=ORIENTED_EDGE('',*,*,#8299,.T.);
#11675=ORIENTED_EDGE('',*,*,#8187,.F.);
#11676=ORIENTED_EDGE('',*,*,#8299,.F.);
#11677=ORIENTED_EDGE('',*,*,#8297,.T.);
#11678=ORIENTED_EDGE('',*,*,#8300,.T.);
#11679=ORIENTED_EDGE('',*,*,#8188,.F.);
#11680=ORIENTED_EDGE('',*,*,#8300,.F.);
#11681=ORIENTED_EDGE('',*,*,#8296,.F.);
#11682=ORIENTED_EDGE('',*,*,#8186,.F.);
#11683=ORIENTED_EDGE('',*,*,#8301,.T.);
#11684=ORIENTED_EDGE('',*,*,#8302,.F.);
#11685=ORIENTED_EDGE('',*,*,#8303,.F.);
#11686=ORIENTED_EDGE('',*,*,#8117,.F.);
#11687=ORIENTED_EDGE('',*,*,#8303,.T.);
#11688=ORIENTED_EDGE('',*,*,#8304,.T.);
#11689=ORIENTED_EDGE('',*,*,#8184,.F.);
#11690=ORIENTED_EDGE('',*,*,#8304,.F.);
#11691=ORIENTED_EDGE('',*,*,#8302,.T.);
#11692=ORIENTED_EDGE('',*,*,#8305,.T.);
#11693=ORIENTED_EDGE('',*,*,#8185,.F.);
#11694=ORIENTED_EDGE('',*,*,#8305,.F.);
#11695=ORIENTED_EDGE('',*,*,#8301,.F.);
#11696=ORIENTED_EDGE('',*,*,#8183,.F.);
#11697=ORIENTED_EDGE('',*,*,#8306,.T.);
#11698=ORIENTED_EDGE('',*,*,#8307,.F.);
#11699=ORIENTED_EDGE('',*,*,#8308,.F.);
#11700=ORIENTED_EDGE('',*,*,#8119,.F.);
#11701=ORIENTED_EDGE('',*,*,#8308,.T.);
#11702=ORIENTED_EDGE('',*,*,#8309,.T.);
#11703=ORIENTED_EDGE('',*,*,#8181,.F.);
#11704=ORIENTED_EDGE('',*,*,#8309,.F.);
#11705=ORIENTED_EDGE('',*,*,#8307,.T.);
#11706=ORIENTED_EDGE('',*,*,#8310,.T.);
#11707=ORIENTED_EDGE('',*,*,#8182,.F.);
#11708=ORIENTED_EDGE('',*,*,#8310,.F.);
#11709=ORIENTED_EDGE('',*,*,#8306,.F.);
#11710=ORIENTED_EDGE('',*,*,#8180,.F.);
#11711=ORIENTED_EDGE('',*,*,#8311,.T.);
#11712=ORIENTED_EDGE('',*,*,#8312,.F.);
#11713=ORIENTED_EDGE('',*,*,#8313,.F.);
#11714=ORIENTED_EDGE('',*,*,#8121,.F.);
#11715=ORIENTED_EDGE('',*,*,#8313,.T.);
#11716=ORIENTED_EDGE('',*,*,#8314,.T.);
#11717=ORIENTED_EDGE('',*,*,#8178,.F.);
#11718=ORIENTED_EDGE('',*,*,#8314,.F.);
#11719=ORIENTED_EDGE('',*,*,#8312,.T.);
#11720=ORIENTED_EDGE('',*,*,#8315,.T.);
#11721=ORIENTED_EDGE('',*,*,#8179,.F.);
#11722=ORIENTED_EDGE('',*,*,#8315,.F.);
#11723=ORIENTED_EDGE('',*,*,#8311,.F.);
#11724=ORIENTED_EDGE('',*,*,#8177,.F.);
#11725=ORIENTED_EDGE('',*,*,#8316,.T.);
#11726=ORIENTED_EDGE('',*,*,#8317,.F.);
#11727=ORIENTED_EDGE('',*,*,#8318,.F.);
#11728=ORIENTED_EDGE('',*,*,#8123,.F.);
#11729=ORIENTED_EDGE('',*,*,#8318,.T.);
#11730=ORIENTED_EDGE('',*,*,#8319,.T.);
#11731=ORIENTED_EDGE('',*,*,#8175,.F.);
#11732=ORIENTED_EDGE('',*,*,#8319,.F.);
#11733=ORIENTED_EDGE('',*,*,#8317,.T.);
#11734=ORIENTED_EDGE('',*,*,#8320,.T.);
#11735=ORIENTED_EDGE('',*,*,#8176,.F.);
#11736=ORIENTED_EDGE('',*,*,#8320,.F.);
#11737=ORIENTED_EDGE('',*,*,#8316,.F.);
#11738=ORIENTED_EDGE('',*,*,#8174,.F.);
#11739=ORIENTED_EDGE('',*,*,#8321,.T.);
#11740=ORIENTED_EDGE('',*,*,#8322,.F.);
#11741=ORIENTED_EDGE('',*,*,#8323,.F.);
#11742=ORIENTED_EDGE('',*,*,#8125,.F.);
#11743=ORIENTED_EDGE('',*,*,#8323,.T.);
#11744=ORIENTED_EDGE('',*,*,#8324,.T.);
#11745=ORIENTED_EDGE('',*,*,#8172,.F.);
#11746=ORIENTED_EDGE('',*,*,#8324,.F.);
#11747=ORIENTED_EDGE('',*,*,#8322,.T.);
#11748=ORIENTED_EDGE('',*,*,#8325,.T.);
#11749=ORIENTED_EDGE('',*,*,#8173,.F.);
#11750=ORIENTED_EDGE('',*,*,#8325,.F.);
#11751=ORIENTED_EDGE('',*,*,#8321,.F.);
#11752=ORIENTED_EDGE('',*,*,#8171,.F.);
#11753=ORIENTED_EDGE('',*,*,#8326,.T.);
#11754=ORIENTED_EDGE('',*,*,#8327,.F.);
#11755=ORIENTED_EDGE('',*,*,#8328,.F.);
#11756=ORIENTED_EDGE('',*,*,#8127,.F.);
#11757=ORIENTED_EDGE('',*,*,#8328,.T.);
#11758=ORIENTED_EDGE('',*,*,#8329,.T.);
#11759=ORIENTED_EDGE('',*,*,#8169,.F.);
#11760=ORIENTED_EDGE('',*,*,#8329,.F.);
#11761=ORIENTED_EDGE('',*,*,#8327,.T.);
#11762=ORIENTED_EDGE('',*,*,#8330,.T.);
#11763=ORIENTED_EDGE('',*,*,#8170,.F.);
#11764=ORIENTED_EDGE('',*,*,#8330,.F.);
#11765=ORIENTED_EDGE('',*,*,#8326,.F.);
#11766=ORIENTED_EDGE('',*,*,#8168,.F.);
#11767=ORIENTED_EDGE('',*,*,#8331,.T.);
#11768=ORIENTED_EDGE('',*,*,#8332,.F.);
#11769=ORIENTED_EDGE('',*,*,#8333,.F.);
#11770=ORIENTED_EDGE('',*,*,#8078,.F.);
#11771=ORIENTED_EDGE('',*,*,#8333,.T.);
#11772=ORIENTED_EDGE('',*,*,#8334,.T.);
#11773=ORIENTED_EDGE('',*,*,#8081,.F.);
#11774=ORIENTED_EDGE('',*,*,#8166,.F.);
#11775=ORIENTED_EDGE('',*,*,#8334,.F.);
#11776=ORIENTED_EDGE('',*,*,#8332,.T.);
#11777=ORIENTED_EDGE('',*,*,#8335,.T.);
#11778=ORIENTED_EDGE('',*,*,#8167,.F.);
#11779=ORIENTED_EDGE('',*,*,#8335,.F.);
#11780=ORIENTED_EDGE('',*,*,#8331,.F.);
#11781=ORIENTED_EDGE('',*,*,#8336,.F.);
#11782=ORIENTED_EDGE('',*,*,#8210,.F.);
#11783=ORIENTED_EDGE('',*,*,#7913,.F.);
#11784=ORIENTED_EDGE('',*,*,#8211,.F.);
#11785=ORIENTED_EDGE('',*,*,#8337,.T.);
#11786=ORIENTED_EDGE('',*,*,#8336,.T.);
#11787=ORIENTED_EDGE('',*,*,#8337,.F.);
#11788=ORIENTED_EDGE('',*,*,#7993,.T.);
#11789=ORIENTED_EDGE('',*,*,#8207,.T.);
#11790=ORIENTED_EDGE('',*,*,#8204,.F.);
#11791=ORIENTED_EDGE('',*,*,#8215,.T.);
#11792=ORIENTED_EDGE('',*,*,#8338,.F.);
#11793=ORIENTED_EDGE('',*,*,#8339,.T.);
#11794=ORIENTED_EDGE('',*,*,#8129,.T.);
#11795=ORIENTED_EDGE('',*,*,#8339,.F.);
#11796=ORIENTED_EDGE('',*,*,#8338,.T.);
#11797=ORIENTED_EDGE('',*,*,#8340,.F.);
#11798=ORIENTED_EDGE('',*,*,#8340,.T.);
#11799=ORIENTED_EDGE('',*,*,#8341,.T.);
#11800=ORIENTED_EDGE('',*,*,#8342,.F.);
#11801=ORIENTED_EDGE('',*,*,#8341,.F.);
#11802=ORIENTED_EDGE('',*,*,#8342,.T.);
#11803=ORIENTED_EDGE('',*,*,#8343,.T.);
#11804=ORIENTED_EDGE('',*,*,#8344,.T.);
#11805=ORIENTED_EDGE('',*,*,#8345,.T.);
#11806=ORIENTED_EDGE('',*,*,#8346,.T.);
#11807=ORIENTED_EDGE('',*,*,#8345,.F.);
#11808=ORIENTED_EDGE('',*,*,#8343,.F.);
#11809=ORIENTED_EDGE('',*,*,#8344,.F.);
#11810=ORIENTED_EDGE('',*,*,#8347,.T.);
#11811=ORIENTED_EDGE('',*,*,#8348,.F.);
#11812=ORIENTED_EDGE('',*,*,#8347,.F.);
#11813=ORIENTED_EDGE('',*,*,#8349,.T.);
#11814=ORIENTED_EDGE('',*,*,#8346,.F.);
#11815=ORIENTED_EDGE('',*,*,#8350,.T.);
#11816=ORIENTED_EDGE('',*,*,#8351,.T.);
#11817=ORIENTED_EDGE('',*,*,#8352,.T.);
#11818=ORIENTED_EDGE('',*,*,#8353,.T.);
#11819=ORIENTED_EDGE('',*,*,#8354,.T.);
#11820=ORIENTED_EDGE('',*,*,#8351,.F.);
#11821=ORIENTED_EDGE('',*,*,#8355,.F.);
#11822=ORIENTED_EDGE('',*,*,#8356,.F.);
#11823=ORIENTED_EDGE('',*,*,#8357,.F.);
#11824=ORIENTED_EDGE('',*,*,#8358,.T.);
#11825=ORIENTED_EDGE('',*,*,#8359,.F.);
#11826=ORIENTED_EDGE('',*,*,#8360,.F.);
#11827=ORIENTED_EDGE('',*,*,#8361,.F.);
#11828=ORIENTED_EDGE('',*,*,#8362,.F.);
#11829=ORIENTED_EDGE('',*,*,#8363,.T.);
#11830=ORIENTED_EDGE('',*,*,#8364,.F.);
#11831=ORIENTED_EDGE('',*,*,#8365,.F.);
#11832=ORIENTED_EDGE('',*,*,#8366,.F.);
#11833=ORIENTED_EDGE('',*,*,#8367,.T.);
#11834=ORIENTED_EDGE('',*,*,#8368,.F.);
#11835=ORIENTED_EDGE('',*,*,#8369,.F.);
#11836=ORIENTED_EDGE('',*,*,#8370,.F.);
#11837=ORIENTED_EDGE('',*,*,#8371,.T.);
#11838=ORIENTED_EDGE('',*,*,#8372,.F.);
#11839=ORIENTED_EDGE('',*,*,#8373,.F.);
#11840=ORIENTED_EDGE('',*,*,#8374,.F.);
#11841=ORIENTED_EDGE('',*,*,#8375,.T.);
#11842=ORIENTED_EDGE('',*,*,#8376,.F.);
#11843=ORIENTED_EDGE('',*,*,#8377,.F.);
#11844=ORIENTED_EDGE('',*,*,#8378,.F.);
#11845=ORIENTED_EDGE('',*,*,#8379,.T.);
#11846=ORIENTED_EDGE('',*,*,#8380,.F.);
#11847=ORIENTED_EDGE('',*,*,#8381,.F.);
#11848=ORIENTED_EDGE('',*,*,#8382,.F.);
#11849=ORIENTED_EDGE('',*,*,#8383,.T.);
#11850=ORIENTED_EDGE('',*,*,#8384,.F.);
#11851=ORIENTED_EDGE('',*,*,#8385,.F.);
#11852=ORIENTED_EDGE('',*,*,#8386,.F.);
#11853=ORIENTED_EDGE('',*,*,#8387,.T.);
#11854=ORIENTED_EDGE('',*,*,#8388,.T.);
#11855=ORIENTED_EDGE('',*,*,#8389,.T.);
#11856=ORIENTED_EDGE('',*,*,#8388,.F.);
#11857=ORIENTED_EDGE('',*,*,#8390,.T.);
#11858=ORIENTED_EDGE('',*,*,#8391,.F.);
#11859=ORIENTED_EDGE('',*,*,#8392,.F.);
#11860=ORIENTED_EDGE('',*,*,#8393,.F.);
#11861=ORIENTED_EDGE('',*,*,#8394,.T.);
#11862=ORIENTED_EDGE('',*,*,#8395,.F.);
#11863=ORIENTED_EDGE('',*,*,#8396,.F.);
#11864=ORIENTED_EDGE('',*,*,#8397,.F.);
#11865=ORIENTED_EDGE('',*,*,#8398,.T.);
#11866=ORIENTED_EDGE('',*,*,#8399,.F.);
#11867=ORIENTED_EDGE('',*,*,#8400,.F.);
#11868=ORIENTED_EDGE('',*,*,#8401,.F.);
#11869=ORIENTED_EDGE('',*,*,#8402,.T.);
#11870=ORIENTED_EDGE('',*,*,#8403,.F.);
#11871=ORIENTED_EDGE('',*,*,#8404,.F.);
#11872=ORIENTED_EDGE('',*,*,#8405,.F.);
#11873=ORIENTED_EDGE('',*,*,#8406,.T.);
#11874=ORIENTED_EDGE('',*,*,#8407,.F.);
#11875=ORIENTED_EDGE('',*,*,#8408,.F.);
#11876=ORIENTED_EDGE('',*,*,#8409,.F.);
#11877=ORIENTED_EDGE('',*,*,#8410,.T.);
#11878=ORIENTED_EDGE('',*,*,#8411,.F.);
#11879=ORIENTED_EDGE('',*,*,#8412,.F.);
#11880=ORIENTED_EDGE('',*,*,#8413,.F.);
#11881=ORIENTED_EDGE('',*,*,#8414,.T.);
#11882=ORIENTED_EDGE('',*,*,#8415,.F.);
#11883=ORIENTED_EDGE('',*,*,#8416,.F.);
#11884=ORIENTED_EDGE('',*,*,#8417,.F.);
#11885=ORIENTED_EDGE('',*,*,#8418,.T.);
#11886=ORIENTED_EDGE('',*,*,#8419,.F.);
#11887=ORIENTED_EDGE('',*,*,#8420,.F.);
#11888=ORIENTED_EDGE('',*,*,#8421,.F.);
#11889=ORIENTED_EDGE('',*,*,#8349,.F.);
#11890=ORIENTED_EDGE('',*,*,#8422,.T.);
#11891=ORIENTED_EDGE('',*,*,#8423,.T.);
#11892=ORIENTED_EDGE('',*,*,#8424,.F.);
#11893=ORIENTED_EDGE('',*,*,#8385,.T.);
#11894=ORIENTED_EDGE('',*,*,#8425,.F.);
#11895=ORIENTED_EDGE('',*,*,#8426,.T.);
#11896=ORIENTED_EDGE('',*,*,#8427,.F.);
#11897=ORIENTED_EDGE('',*,*,#8381,.T.);
#11898=ORIENTED_EDGE('',*,*,#8428,.F.);
#11899=ORIENTED_EDGE('',*,*,#8429,.T.);
#11900=ORIENTED_EDGE('',*,*,#8430,.F.);
#11901=ORIENTED_EDGE('',*,*,#8377,.T.);
#11902=ORIENTED_EDGE('',*,*,#8431,.F.);
#11903=ORIENTED_EDGE('',*,*,#8432,.T.);
#11904=ORIENTED_EDGE('',*,*,#8433,.F.);
#11905=ORIENTED_EDGE('',*,*,#8373,.T.);
#11906=ORIENTED_EDGE('',*,*,#8434,.F.);
#11907=ORIENTED_EDGE('',*,*,#8435,.T.);
#11908=ORIENTED_EDGE('',*,*,#8436,.F.);
#11909=ORIENTED_EDGE('',*,*,#8369,.T.);
#11910=ORIENTED_EDGE('',*,*,#8437,.F.);
#11911=ORIENTED_EDGE('',*,*,#8438,.T.);
#11912=ORIENTED_EDGE('',*,*,#8439,.F.);
#11913=ORIENTED_EDGE('',*,*,#8365,.T.);
#11914=ORIENTED_EDGE('',*,*,#8440,.F.);
#11915=ORIENTED_EDGE('',*,*,#8441,.T.);
#11916=ORIENTED_EDGE('',*,*,#8442,.F.);
#11917=ORIENTED_EDGE('',*,*,#8361,.T.);
#11918=ORIENTED_EDGE('',*,*,#8443,.F.);
#11919=ORIENTED_EDGE('',*,*,#8355,.T.);
#11920=ORIENTED_EDGE('',*,*,#8350,.F.);
#11921=ORIENTED_EDGE('',*,*,#8444,.T.);
#11922=ORIENTED_EDGE('',*,*,#8445,.F.);
#11923=ORIENTED_EDGE('',*,*,#8420,.T.);
#11924=ORIENTED_EDGE('',*,*,#8446,.F.);
#11925=ORIENTED_EDGE('',*,*,#8447,.T.);
#11926=ORIENTED_EDGE('',*,*,#8448,.F.);
#11927=ORIENTED_EDGE('',*,*,#8416,.T.);
#11928=ORIENTED_EDGE('',*,*,#8449,.F.);
#11929=ORIENTED_EDGE('',*,*,#8450,.T.);
#11930=ORIENTED_EDGE('',*,*,#8451,.F.);
#11931=ORIENTED_EDGE('',*,*,#8412,.T.);
#11932=ORIENTED_EDGE('',*,*,#8452,.F.);
#11933=ORIENTED_EDGE('',*,*,#8453,.T.);
#11934=ORIENTED_EDGE('',*,*,#8454,.F.);
#11935=ORIENTED_EDGE('',*,*,#8408,.T.);
#11936=ORIENTED_EDGE('',*,*,#8455,.F.);
#11937=ORIENTED_EDGE('',*,*,#8456,.T.);
#11938=ORIENTED_EDGE('',*,*,#8457,.F.);
#11939=ORIENTED_EDGE('',*,*,#8404,.T.);
#11940=ORIENTED_EDGE('',*,*,#8458,.F.);
#11941=ORIENTED_EDGE('',*,*,#8459,.T.);
#11942=ORIENTED_EDGE('',*,*,#8460,.F.);
#11943=ORIENTED_EDGE('',*,*,#8400,.T.);
#11944=ORIENTED_EDGE('',*,*,#8461,.F.);
#11945=ORIENTED_EDGE('',*,*,#8462,.T.);
#11946=ORIENTED_EDGE('',*,*,#8463,.F.);
#11947=ORIENTED_EDGE('',*,*,#8396,.T.);
#11948=ORIENTED_EDGE('',*,*,#8464,.F.);
#11949=ORIENTED_EDGE('',*,*,#8465,.T.);
#11950=ORIENTED_EDGE('',*,*,#8466,.F.);
#11951=ORIENTED_EDGE('',*,*,#8392,.T.);
#11952=ORIENTED_EDGE('',*,*,#8467,.F.);
#11953=ORIENTED_EDGE('',*,*,#8468,.T.);
#11954=ORIENTED_EDGE('',*,*,#8422,.F.);
#11955=ORIENTED_EDGE('',*,*,#8445,.T.);
#11956=ORIENTED_EDGE('',*,*,#8469,.T.);
#11957=ORIENTED_EDGE('',*,*,#8470,.T.);
#11958=ORIENTED_EDGE('',*,*,#8421,.T.);
#11959=ORIENTED_EDGE('',*,*,#8446,.T.);
#11960=ORIENTED_EDGE('',*,*,#8419,.T.);
#11961=ORIENTED_EDGE('',*,*,#8471,.T.);
#11962=ORIENTED_EDGE('',*,*,#8472,.T.);
#11963=ORIENTED_EDGE('',*,*,#8448,.T.);
#11964=ORIENTED_EDGE('',*,*,#8473,.T.);
#11965=ORIENTED_EDGE('',*,*,#8474,.T.);
#11966=ORIENTED_EDGE('',*,*,#8417,.T.);
#11967=ORIENTED_EDGE('',*,*,#8449,.T.);
#11968=ORIENTED_EDGE('',*,*,#8415,.T.);
#11969=ORIENTED_EDGE('',*,*,#8475,.T.);
#11970=ORIENTED_EDGE('',*,*,#8476,.T.);
#11971=ORIENTED_EDGE('',*,*,#8451,.T.);
#11972=ORIENTED_EDGE('',*,*,#8477,.T.);
#11973=ORIENTED_EDGE('',*,*,#8478,.T.);
#11974=ORIENTED_EDGE('',*,*,#8413,.T.);
#11975=ORIENTED_EDGE('',*,*,#8452,.T.);
#11976=ORIENTED_EDGE('',*,*,#8411,.T.);
#11977=ORIENTED_EDGE('',*,*,#8479,.T.);
#11978=ORIENTED_EDGE('',*,*,#8480,.T.);
#11979=ORIENTED_EDGE('',*,*,#8454,.T.);
#11980=ORIENTED_EDGE('',*,*,#8481,.T.);
#11981=ORIENTED_EDGE('',*,*,#8482,.T.);
#11982=ORIENTED_EDGE('',*,*,#8409,.T.);
#11983=ORIENTED_EDGE('',*,*,#8455,.T.);
#11984=ORIENTED_EDGE('',*,*,#8407,.T.);
#11985=ORIENTED_EDGE('',*,*,#8483,.T.);
#11986=ORIENTED_EDGE('',*,*,#8484,.T.);
#11987=ORIENTED_EDGE('',*,*,#8457,.T.);
#11988=ORIENTED_EDGE('',*,*,#8485,.T.);
#11989=ORIENTED_EDGE('',*,*,#8486,.T.);
#11990=ORIENTED_EDGE('',*,*,#8405,.T.);
#11991=ORIENTED_EDGE('',*,*,#8458,.T.);
#11992=ORIENTED_EDGE('',*,*,#8403,.T.);
#11993=ORIENTED_EDGE('',*,*,#8487,.T.);
#11994=ORIENTED_EDGE('',*,*,#8488,.T.);
#11995=ORIENTED_EDGE('',*,*,#8460,.T.);
#11996=ORIENTED_EDGE('',*,*,#8489,.T.);
#11997=ORIENTED_EDGE('',*,*,#8490,.T.);
#11998=ORIENTED_EDGE('',*,*,#8401,.T.);
#11999=ORIENTED_EDGE('',*,*,#8461,.T.);
#12000=ORIENTED_EDGE('',*,*,#8399,.T.);
#12001=ORIENTED_EDGE('',*,*,#8491,.T.);
#12002=ORIENTED_EDGE('',*,*,#8492,.T.);
#12003=ORIENTED_EDGE('',*,*,#8463,.T.);
#12004=ORIENTED_EDGE('',*,*,#8493,.T.);
#12005=ORIENTED_EDGE('',*,*,#8494,.T.);
#12006=ORIENTED_EDGE('',*,*,#8397,.T.);
#12007=ORIENTED_EDGE('',*,*,#8464,.T.);
#12008=ORIENTED_EDGE('',*,*,#8395,.T.);
#12009=ORIENTED_EDGE('',*,*,#8495,.T.);
#12010=ORIENTED_EDGE('',*,*,#8496,.T.);
#12011=ORIENTED_EDGE('',*,*,#8466,.T.);
#12012=ORIENTED_EDGE('',*,*,#8497,.T.);
#12013=ORIENTED_EDGE('',*,*,#8498,.T.);
#12014=ORIENTED_EDGE('',*,*,#8393,.T.);
#12015=ORIENTED_EDGE('',*,*,#8467,.T.);
#12016=ORIENTED_EDGE('',*,*,#8391,.T.);
#12017=ORIENTED_EDGE('',*,*,#8499,.T.);
#12018=ORIENTED_EDGE('',*,*,#8500,.T.);
#12019=ORIENTED_EDGE('',*,*,#8424,.T.);
#12020=ORIENTED_EDGE('',*,*,#8501,.T.);
#12021=ORIENTED_EDGE('',*,*,#8502,.T.);
#12022=ORIENTED_EDGE('',*,*,#8386,.T.);
#12023=ORIENTED_EDGE('',*,*,#8425,.T.);
#12024=ORIENTED_EDGE('',*,*,#8384,.T.);
#12025=ORIENTED_EDGE('',*,*,#8503,.T.);
#12026=ORIENTED_EDGE('',*,*,#8504,.T.);
#12027=ORIENTED_EDGE('',*,*,#8427,.T.);
#12028=ORIENTED_EDGE('',*,*,#8505,.T.);
#12029=ORIENTED_EDGE('',*,*,#8506,.T.);
#12030=ORIENTED_EDGE('',*,*,#8382,.T.);
#12031=ORIENTED_EDGE('',*,*,#8428,.T.);
#12032=ORIENTED_EDGE('',*,*,#8380,.T.);
#12033=ORIENTED_EDGE('',*,*,#8507,.T.);
#12034=ORIENTED_EDGE('',*,*,#8508,.T.);
#12035=ORIENTED_EDGE('',*,*,#8430,.T.);
#12036=ORIENTED_EDGE('',*,*,#8509,.T.);
#12037=ORIENTED_EDGE('',*,*,#8510,.T.);
#12038=ORIENTED_EDGE('',*,*,#8378,.T.);
#12039=ORIENTED_EDGE('',*,*,#8431,.T.);
#12040=ORIENTED_EDGE('',*,*,#8376,.T.);
#12041=ORIENTED_EDGE('',*,*,#8511,.T.);
#12042=ORIENTED_EDGE('',*,*,#8512,.T.);
#12043=ORIENTED_EDGE('',*,*,#8433,.T.);
#12044=ORIENTED_EDGE('',*,*,#8513,.T.);
#12045=ORIENTED_EDGE('',*,*,#8514,.T.);
#12046=ORIENTED_EDGE('',*,*,#8374,.T.);
#12047=ORIENTED_EDGE('',*,*,#8434,.T.);
#12048=ORIENTED_EDGE('',*,*,#8372,.T.);
#12049=ORIENTED_EDGE('',*,*,#8515,.T.);
#12050=ORIENTED_EDGE('',*,*,#8516,.T.);
#12051=ORIENTED_EDGE('',*,*,#8436,.T.);
#12052=ORIENTED_EDGE('',*,*,#8517,.T.);
#12053=ORIENTED_EDGE('',*,*,#8518,.T.);
#12054=ORIENTED_EDGE('',*,*,#8370,.T.);
#12055=ORIENTED_EDGE('',*,*,#8437,.T.);
#12056=ORIENTED_EDGE('',*,*,#8368,.T.);
#12057=ORIENTED_EDGE('',*,*,#8519,.T.);
#12058=ORIENTED_EDGE('',*,*,#8520,.T.);
#12059=ORIENTED_EDGE('',*,*,#8439,.T.);
#12060=ORIENTED_EDGE('',*,*,#8521,.T.);
#12061=ORIENTED_EDGE('',*,*,#8522,.T.);
#12062=ORIENTED_EDGE('',*,*,#8366,.T.);
#12063=ORIENTED_EDGE('',*,*,#8440,.T.);
#12064=ORIENTED_EDGE('',*,*,#8364,.T.);
#12065=ORIENTED_EDGE('',*,*,#8523,.T.);
#12066=ORIENTED_EDGE('',*,*,#8524,.T.);
#12067=ORIENTED_EDGE('',*,*,#8442,.T.);
#12068=ORIENTED_EDGE('',*,*,#8525,.T.);
#12069=ORIENTED_EDGE('',*,*,#8526,.T.);
#12070=ORIENTED_EDGE('',*,*,#8362,.T.);
#12071=ORIENTED_EDGE('',*,*,#8527,.T.);
#12072=ORIENTED_EDGE('',*,*,#8528,.T.);
#12073=ORIENTED_EDGE('',*,*,#8356,.T.);
#12074=ORIENTED_EDGE('',*,*,#8443,.T.);
#12075=ORIENTED_EDGE('',*,*,#8360,.T.);
#12076=ORIENTED_EDGE('',*,*,#8529,.T.);
#12077=ORIENTED_EDGE('',*,*,#8530,.T.);
#12078=ORIENTED_EDGE('',*,*,#8531,.T.);
#12079=ORIENTED_EDGE('',*,*,#8357,.T.);
#12080=ORIENTED_EDGE('',*,*,#8528,.F.);
#12081=ORIENTED_EDGE('',*,*,#8359,.T.);
#12082=ORIENTED_EDGE('',*,*,#8532,.T.);
#12083=ORIENTED_EDGE('',*,*,#8533,.T.);
#12084=ORIENTED_EDGE('',*,*,#8529,.F.);
#12085=ORIENTED_EDGE('',*,*,#8530,.F.);
#12086=ORIENTED_EDGE('',*,*,#8527,.F.);
#12087=ORIENTED_EDGE('',*,*,#8533,.F.);
#12088=ORIENTED_EDGE('',*,*,#8534,.F.);
#12089=ORIENTED_EDGE('',*,*,#8348,.T.);
#12090=ORIENTED_EDGE('',*,*,#8535,.T.);
#12091=ORIENTED_EDGE('',*,*,#8536,.T.);
#12092=ORIENTED_EDGE('',*,*,#8535,.F.);
#12093=ORIENTED_EDGE('',*,*,#8537,.F.);
#12094=ORIENTED_EDGE('',*,*,#8538,.F.);
#12095=ORIENTED_EDGE('',*,*,#8539,.F.);
#12096=ORIENTED_EDGE('',*,*,#8540,.F.);
#12097=ORIENTED_EDGE('',*,*,#8541,.F.);
#12098=ORIENTED_EDGE('',*,*,#8542,.F.);
#12099=ORIENTED_EDGE('',*,*,#8536,.F.);
#12100=ORIENTED_EDGE('',*,*,#8543,.T.);
#12101=ORIENTED_EDGE('',*,*,#8544,.T.);
#12102=ORIENTED_EDGE('',*,*,#8545,.T.);
#12103=ORIENTED_EDGE('',*,*,#8546,.F.);
#12104=ORIENTED_EDGE('',*,*,#8547,.T.);
#12105=ORIENTED_EDGE('',*,*,#8548,.T.);
#12106=ORIENTED_EDGE('',*,*,#8549,.T.);
#12107=ORIENTED_EDGE('',*,*,#8544,.F.);
#12108=ORIENTED_EDGE('',*,*,#8550,.T.);
#12109=ORIENTED_EDGE('',*,*,#8551,.T.);
#12110=ORIENTED_EDGE('',*,*,#8552,.T.);
#12111=ORIENTED_EDGE('',*,*,#8553,.T.);
#12112=ORIENTED_EDGE('',*,*,#8554,.T.);
#12113=ORIENTED_EDGE('',*,*,#8551,.F.);
#12114=ORIENTED_EDGE('',*,*,#8555,.T.);
#12115=ORIENTED_EDGE('',*,*,#8556,.T.);
#12116=ORIENTED_EDGE('',*,*,#8557,.T.);
#12117=ORIENTED_EDGE('',*,*,#8553,.F.);
#12118=ORIENTED_EDGE('',*,*,#8558,.T.);
#12119=ORIENTED_EDGE('',*,*,#8548,.F.);
#12120=ORIENTED_EDGE('',*,*,#8559,.T.);
#12121=ORIENTED_EDGE('',*,*,#8556,.F.);
#12122=ORIENTED_EDGE('',*,*,#8560,.T.);
#12123=ORIENTED_EDGE('',*,*,#8546,.T.);
#12124=ORIENTED_EDGE('',*,*,#8549,.F.);
#12125=ORIENTED_EDGE('',*,*,#8561,.T.);
#12126=ORIENTED_EDGE('',*,*,#8542,.T.);
#12127=ORIENTED_EDGE('',*,*,#8562,.F.);
#12128=ORIENTED_EDGE('',*,*,#8558,.F.);
#12129=ORIENTED_EDGE('',*,*,#8563,.T.);
#12130=ORIENTED_EDGE('',*,*,#8537,.T.);
#12131=ORIENTED_EDGE('',*,*,#8561,.F.);
#12132=ORIENTED_EDGE('',*,*,#8552,.F.);
#12133=ORIENTED_EDGE('',*,*,#8564,.T.);
#12134=ORIENTED_EDGE('',*,*,#8538,.T.);
#12135=ORIENTED_EDGE('',*,*,#8563,.F.);
#12136=ORIENTED_EDGE('',*,*,#8565,.F.);
#12137=ORIENTED_EDGE('',*,*,#8550,.F.);
#12138=ORIENTED_EDGE('',*,*,#8557,.F.);
#12139=ORIENTED_EDGE('',*,*,#8547,.F.);
#12140=ORIENTED_EDGE('',*,*,#8543,.F.);
#12141=ORIENTED_EDGE('',*,*,#8560,.F.);
#12142=ORIENTED_EDGE('',*,*,#8555,.F.);
#12143=ORIENTED_EDGE('',*,*,#8554,.F.);
#12144=ORIENTED_EDGE('',*,*,#8566,.T.);
#12145=ORIENTED_EDGE('',*,*,#8539,.T.);
#12146=ORIENTED_EDGE('',*,*,#8564,.F.);
#12147=ORIENTED_EDGE('',*,*,#8559,.F.);
#12148=ORIENTED_EDGE('',*,*,#8567,.T.);
#12149=ORIENTED_EDGE('',*,*,#8540,.T.);
#12150=ORIENTED_EDGE('',*,*,#8566,.F.);
#12151=ORIENTED_EDGE('',*,*,#8545,.F.);
#12152=ORIENTED_EDGE('',*,*,#8562,.T.);
#12153=ORIENTED_EDGE('',*,*,#8541,.T.);
#12154=ORIENTED_EDGE('',*,*,#8567,.F.);
#12155=ORIENTED_EDGE('',*,*,#8358,.F.);
#12156=ORIENTED_EDGE('',*,*,#8531,.F.);
#12157=ORIENTED_EDGE('',*,*,#8534,.T.);
#12158=ORIENTED_EDGE('',*,*,#8532,.F.);
#12159=ORIENTED_EDGE('',*,*,#8524,.F.);
#12160=ORIENTED_EDGE('',*,*,#8568,.F.);
#12161=ORIENTED_EDGE('',*,*,#8525,.F.);
#12162=ORIENTED_EDGE('',*,*,#8441,.F.);
#12163=ORIENTED_EDGE('',*,*,#8363,.F.);
#12164=ORIENTED_EDGE('',*,*,#8526,.F.);
#12165=ORIENTED_EDGE('',*,*,#8568,.T.);
#12166=ORIENTED_EDGE('',*,*,#8523,.F.);
#12167=ORIENTED_EDGE('',*,*,#8367,.F.);
#12168=ORIENTED_EDGE('',*,*,#8522,.F.);
#12169=ORIENTED_EDGE('',*,*,#8569,.T.);
#12170=ORIENTED_EDGE('',*,*,#8519,.F.);
#12171=ORIENTED_EDGE('',*,*,#8520,.F.);
#12172=ORIENTED_EDGE('',*,*,#8569,.F.);
#12173=ORIENTED_EDGE('',*,*,#8521,.F.);
#12174=ORIENTED_EDGE('',*,*,#8438,.F.);
#12175=ORIENTED_EDGE('',*,*,#8516,.F.);
#12176=ORIENTED_EDGE('',*,*,#8570,.F.);
#12177=ORIENTED_EDGE('',*,*,#8517,.F.);
#12178=ORIENTED_EDGE('',*,*,#8435,.F.);
#12179=ORIENTED_EDGE('',*,*,#8371,.F.);
#12180=ORIENTED_EDGE('',*,*,#8518,.F.);
#12181=ORIENTED_EDGE('',*,*,#8570,.T.);
#12182=ORIENTED_EDGE('',*,*,#8515,.F.);
#12183=ORIENTED_EDGE('',*,*,#8375,.F.);
#12184=ORIENTED_EDGE('',*,*,#8514,.F.);
#12185=ORIENTED_EDGE('',*,*,#8571,.T.);
#12186=ORIENTED_EDGE('',*,*,#8511,.F.);
#12187=ORIENTED_EDGE('',*,*,#8512,.F.);
#12188=ORIENTED_EDGE('',*,*,#8571,.F.);
#12189=ORIENTED_EDGE('',*,*,#8513,.F.);
#12190=ORIENTED_EDGE('',*,*,#8432,.F.);
#12191=ORIENTED_EDGE('',*,*,#8508,.F.);
#12192=ORIENTED_EDGE('',*,*,#8572,.F.);
#12193=ORIENTED_EDGE('',*,*,#8509,.F.);
#12194=ORIENTED_EDGE('',*,*,#8429,.F.);
#12195=ORIENTED_EDGE('',*,*,#8379,.F.);
#12196=ORIENTED_EDGE('',*,*,#8510,.F.);
#12197=ORIENTED_EDGE('',*,*,#8572,.T.);
#12198=ORIENTED_EDGE('',*,*,#8507,.F.);
#12199=ORIENTED_EDGE('',*,*,#8383,.F.);
#12200=ORIENTED_EDGE('',*,*,#8506,.F.);
#12201=ORIENTED_EDGE('',*,*,#8573,.T.);
#12202=ORIENTED_EDGE('',*,*,#8503,.F.);
#12203=ORIENTED_EDGE('',*,*,#8504,.F.);
#12204=ORIENTED_EDGE('',*,*,#8573,.F.);
#12205=ORIENTED_EDGE('',*,*,#8505,.F.);
#12206=ORIENTED_EDGE('',*,*,#8426,.F.);
#12207=ORIENTED_EDGE('',*,*,#8500,.F.);
#12208=ORIENTED_EDGE('',*,*,#8574,.F.);
#12209=ORIENTED_EDGE('',*,*,#8501,.F.);
#12210=ORIENTED_EDGE('',*,*,#8423,.F.);
#12211=ORIENTED_EDGE('',*,*,#8468,.F.);
#12212=ORIENTED_EDGE('',*,*,#8387,.F.);
#12213=ORIENTED_EDGE('',*,*,#8502,.F.);
#12214=ORIENTED_EDGE('',*,*,#8574,.T.);
#12215=ORIENTED_EDGE('',*,*,#8499,.F.);
#12216=ORIENTED_EDGE('',*,*,#8390,.F.);
#12217=ORIENTED_EDGE('',*,*,#8394,.F.);
#12218=ORIENTED_EDGE('',*,*,#8498,.F.);
#12219=ORIENTED_EDGE('',*,*,#8575,.T.);
#12220=ORIENTED_EDGE('',*,*,#8495,.F.);
#12221=ORIENTED_EDGE('',*,*,#8496,.F.);
#12222=ORIENTED_EDGE('',*,*,#8575,.F.);
#12223=ORIENTED_EDGE('',*,*,#8497,.F.);
#12224=ORIENTED_EDGE('',*,*,#8465,.F.);
#12225=ORIENTED_EDGE('',*,*,#8492,.F.);
#12226=ORIENTED_EDGE('',*,*,#8576,.F.);
#12227=ORIENTED_EDGE('',*,*,#8493,.F.);
#12228=ORIENTED_EDGE('',*,*,#8462,.F.);
#12229=ORIENTED_EDGE('',*,*,#8398,.F.);
#12230=ORIENTED_EDGE('',*,*,#8494,.F.);
#12231=ORIENTED_EDGE('',*,*,#8576,.T.);
#12232=ORIENTED_EDGE('',*,*,#8491,.F.);
#12233=ORIENTED_EDGE('',*,*,#8402,.F.);
#12234=ORIENTED_EDGE('',*,*,#8490,.F.);
#12235=ORIENTED_EDGE('',*,*,#8577,.T.);
#12236=ORIENTED_EDGE('',*,*,#8487,.F.);
#12237=ORIENTED_EDGE('',*,*,#8488,.F.);
#12238=ORIENTED_EDGE('',*,*,#8577,.F.);
#12239=ORIENTED_EDGE('',*,*,#8489,.F.);
#12240=ORIENTED_EDGE('',*,*,#8459,.F.);
#12241=ORIENTED_EDGE('',*,*,#8484,.F.);
#12242=ORIENTED_EDGE('',*,*,#8578,.F.);
#12243=ORIENTED_EDGE('',*,*,#8485,.F.);
#12244=ORIENTED_EDGE('',*,*,#8456,.F.);
#12245=ORIENTED_EDGE('',*,*,#8406,.F.);
#12246=ORIENTED_EDGE('',*,*,#8486,.F.);
#12247=ORIENTED_EDGE('',*,*,#8578,.T.);
#12248=ORIENTED_EDGE('',*,*,#8483,.F.);
#12249=ORIENTED_EDGE('',*,*,#8410,.F.);
#12250=ORIENTED_EDGE('',*,*,#8482,.F.);
#12251=ORIENTED_EDGE('',*,*,#8579,.T.);
#12252=ORIENTED_EDGE('',*,*,#8479,.F.);
#12253=ORIENTED_EDGE('',*,*,#8480,.F.);
#12254=ORIENTED_EDGE('',*,*,#8579,.F.);
#12255=ORIENTED_EDGE('',*,*,#8481,.F.);
#12256=ORIENTED_EDGE('',*,*,#8453,.F.);
#12257=ORIENTED_EDGE('',*,*,#8476,.F.);
#12258=ORIENTED_EDGE('',*,*,#8580,.F.);
#12259=ORIENTED_EDGE('',*,*,#8477,.F.);
#12260=ORIENTED_EDGE('',*,*,#8450,.F.);
#12261=ORIENTED_EDGE('',*,*,#8414,.F.);
#12262=ORIENTED_EDGE('',*,*,#8478,.F.);
#12263=ORIENTED_EDGE('',*,*,#8580,.T.);
#12264=ORIENTED_EDGE('',*,*,#8475,.F.);
#12265=ORIENTED_EDGE('',*,*,#8418,.F.);
#12266=ORIENTED_EDGE('',*,*,#8474,.F.);
#12267=ORIENTED_EDGE('',*,*,#8581,.T.);
#12268=ORIENTED_EDGE('',*,*,#8471,.F.);
#12269=ORIENTED_EDGE('',*,*,#8472,.F.);
#12270=ORIENTED_EDGE('',*,*,#8581,.F.);
#12271=ORIENTED_EDGE('',*,*,#8473,.F.);
#12272=ORIENTED_EDGE('',*,*,#8447,.F.);
#12273=ORIENTED_EDGE('',*,*,#8353,.F.);
#12274=ORIENTED_EDGE('',*,*,#8582,.F.);
#12275=ORIENTED_EDGE('',*,*,#8469,.F.);
#12276=ORIENTED_EDGE('',*,*,#8444,.F.);
#12277=ORIENTED_EDGE('',*,*,#8354,.F.);
#12278=ORIENTED_EDGE('',*,*,#8470,.F.);
#12279=ORIENTED_EDGE('',*,*,#8582,.T.);
#12280=ORIENTED_EDGE('',*,*,#8352,.F.);
#12281=ORIENTED_EDGE('',*,*,#8389,.F.);
#12282=ORIENTED_EDGE('',*,*,#8583,.T.);
#12283=ORIENTED_EDGE('',*,*,#8565,.T.);
#12284=ORIENTED_EDGE('',*,*,#8583,.F.);
#12285=ORIENTED_EDGE('',*,*,#8584,.F.);
#12286=ORIENTED_EDGE('',*,*,#8585,.T.);
#12287=ORIENTED_EDGE('',*,*,#8586,.T.);
#12288=ORIENTED_EDGE('',*,*,#8587,.T.);
#12289=ORIENTED_EDGE('',*,*,#8588,.F.);
#12290=ORIENTED_EDGE('',*,*,#8589,.T.);
#12291=ORIENTED_EDGE('',*,*,#8584,.T.);
#12292=ORIENTED_EDGE('',*,*,#8590,.T.);
#12293=ORIENTED_EDGE('',*,*,#8591,.F.);
#12294=ORIENTED_EDGE('',*,*,#8592,.T.);
#12295=ORIENTED_EDGE('',*,*,#8588,.T.);
#12296=ORIENTED_EDGE('',*,*,#8593,.T.);
#12297=ORIENTED_EDGE('',*,*,#8594,.F.);
#12298=ORIENTED_EDGE('',*,*,#8595,.T.);
#12299=ORIENTED_EDGE('',*,*,#8591,.T.);
#12300=ORIENTED_EDGE('',*,*,#8596,.T.);
#12301=ORIENTED_EDGE('',*,*,#8597,.F.);
#12302=ORIENTED_EDGE('',*,*,#8598,.T.);
#12303=ORIENTED_EDGE('',*,*,#8594,.T.);
#12304=ORIENTED_EDGE('',*,*,#8599,.T.);
#12305=ORIENTED_EDGE('',*,*,#8600,.F.);
#12306=ORIENTED_EDGE('',*,*,#8601,.T.);
#12307=ORIENTED_EDGE('',*,*,#8597,.T.);
#12308=ORIENTED_EDGE('',*,*,#8602,.T.);
#12309=ORIENTED_EDGE('',*,*,#8603,.F.);
#12310=ORIENTED_EDGE('',*,*,#8604,.T.);
#12311=ORIENTED_EDGE('',*,*,#8600,.T.);
#12312=ORIENTED_EDGE('',*,*,#8605,.T.);
#12313=ORIENTED_EDGE('',*,*,#8606,.F.);
#12314=ORIENTED_EDGE('',*,*,#8607,.T.);
#12315=ORIENTED_EDGE('',*,*,#8603,.T.);
#12316=ORIENTED_EDGE('',*,*,#8608,.T.);
#12317=ORIENTED_EDGE('',*,*,#8609,.F.);
#12318=ORIENTED_EDGE('',*,*,#8610,.T.);
#12319=ORIENTED_EDGE('',*,*,#8606,.T.);
#12320=ORIENTED_EDGE('',*,*,#8611,.T.);
#12321=ORIENTED_EDGE('',*,*,#8612,.F.);
#12322=ORIENTED_EDGE('',*,*,#8613,.T.);
#12323=ORIENTED_EDGE('',*,*,#8609,.T.);
#12324=ORIENTED_EDGE('',*,*,#8614,.T.);
#12325=ORIENTED_EDGE('',*,*,#8615,.F.);
#12326=ORIENTED_EDGE('',*,*,#8616,.T.);
#12327=ORIENTED_EDGE('',*,*,#8612,.T.);
#12328=ORIENTED_EDGE('',*,*,#8617,.T.);
#12329=ORIENTED_EDGE('',*,*,#8618,.F.);
#12330=ORIENTED_EDGE('',*,*,#8619,.T.);
#12331=ORIENTED_EDGE('',*,*,#8615,.T.);
#12332=ORIENTED_EDGE('',*,*,#8620,.T.);
#12333=ORIENTED_EDGE('',*,*,#8621,.F.);
#12334=ORIENTED_EDGE('',*,*,#8622,.T.);
#12335=ORIENTED_EDGE('',*,*,#8618,.T.);
#12336=ORIENTED_EDGE('',*,*,#8623,.T.);
#12337=ORIENTED_EDGE('',*,*,#8624,.F.);
#12338=ORIENTED_EDGE('',*,*,#8625,.T.);
#12339=ORIENTED_EDGE('',*,*,#8621,.T.);
#12340=ORIENTED_EDGE('',*,*,#8626,.T.);
#12341=ORIENTED_EDGE('',*,*,#8627,.F.);
#12342=ORIENTED_EDGE('',*,*,#8628,.T.);
#12343=ORIENTED_EDGE('',*,*,#8624,.T.);
#12344=ORIENTED_EDGE('',*,*,#8629,.T.);
#12345=ORIENTED_EDGE('',*,*,#8630,.F.);
#12346=ORIENTED_EDGE('',*,*,#8631,.T.);
#12347=ORIENTED_EDGE('',*,*,#8627,.T.);
#12348=ORIENTED_EDGE('',*,*,#8632,.T.);
#12349=ORIENTED_EDGE('',*,*,#8633,.F.);
#12350=ORIENTED_EDGE('',*,*,#8634,.T.);
#12351=ORIENTED_EDGE('',*,*,#8630,.T.);
#12352=ORIENTED_EDGE('',*,*,#8635,.T.);
#12353=ORIENTED_EDGE('',*,*,#8636,.F.);
#12354=ORIENTED_EDGE('',*,*,#8637,.T.);
#12355=ORIENTED_EDGE('',*,*,#8633,.T.);
#12356=ORIENTED_EDGE('',*,*,#8638,.T.);
#12357=ORIENTED_EDGE('',*,*,#8639,.F.);
#12358=ORIENTED_EDGE('',*,*,#8640,.T.);
#12359=ORIENTED_EDGE('',*,*,#8636,.T.);
#12360=ORIENTED_EDGE('',*,*,#8641,.T.);
#12361=ORIENTED_EDGE('',*,*,#8642,.F.);
#12362=ORIENTED_EDGE('',*,*,#8643,.T.);
#12363=ORIENTED_EDGE('',*,*,#8639,.T.);
#12364=ORIENTED_EDGE('',*,*,#8644,.T.);
#12365=ORIENTED_EDGE('',*,*,#8645,.F.);
#12366=ORIENTED_EDGE('',*,*,#8646,.T.);
#12367=ORIENTED_EDGE('',*,*,#8642,.T.);
#12368=ORIENTED_EDGE('',*,*,#8647,.T.);
#12369=ORIENTED_EDGE('',*,*,#8648,.F.);
#12370=ORIENTED_EDGE('',*,*,#8649,.T.);
#12371=ORIENTED_EDGE('',*,*,#8645,.T.);
#12372=ORIENTED_EDGE('',*,*,#8650,.T.);
#12373=ORIENTED_EDGE('',*,*,#8651,.F.);
#12374=ORIENTED_EDGE('',*,*,#8652,.T.);
#12375=ORIENTED_EDGE('',*,*,#8648,.T.);
#12376=ORIENTED_EDGE('',*,*,#8653,.T.);
#12377=ORIENTED_EDGE('',*,*,#8654,.F.);
#12378=ORIENTED_EDGE('',*,*,#8655,.T.);
#12379=ORIENTED_EDGE('',*,*,#8656,.F.);
#12380=ORIENTED_EDGE('',*,*,#8657,.F.);
#12381=ORIENTED_EDGE('',*,*,#8658,.F.);
#12382=ORIENTED_EDGE('',*,*,#8659,.T.);
#12383=ORIENTED_EDGE('',*,*,#8654,.T.);
#12384=ORIENTED_EDGE('',*,*,#8660,.F.);
#12385=ORIENTED_EDGE('',*,*,#8661,.F.);
#12386=ORIENTED_EDGE('',*,*,#8662,.T.);
#12387=ORIENTED_EDGE('',*,*,#8658,.T.);
#12388=ORIENTED_EDGE('',*,*,#8663,.F.);
#12389=ORIENTED_EDGE('',*,*,#8664,.F.);
#12390=ORIENTED_EDGE('',*,*,#8665,.T.);
#12391=ORIENTED_EDGE('',*,*,#8661,.T.);
#12392=ORIENTED_EDGE('',*,*,#8666,.F.);
#12393=ORIENTED_EDGE('',*,*,#8667,.F.);
#12394=ORIENTED_EDGE('',*,*,#8668,.T.);
#12395=ORIENTED_EDGE('',*,*,#8664,.T.);
#12396=ORIENTED_EDGE('',*,*,#8669,.F.);
#12397=ORIENTED_EDGE('',*,*,#8670,.F.);
#12398=ORIENTED_EDGE('',*,*,#8671,.T.);
#12399=ORIENTED_EDGE('',*,*,#8667,.T.);
#12400=ORIENTED_EDGE('',*,*,#8672,.F.);
#12401=ORIENTED_EDGE('',*,*,#8673,.F.);
#12402=ORIENTED_EDGE('',*,*,#8674,.T.);
#12403=ORIENTED_EDGE('',*,*,#8670,.T.);
#12404=ORIENTED_EDGE('',*,*,#8675,.F.);
#12405=ORIENTED_EDGE('',*,*,#8676,.F.);
#12406=ORIENTED_EDGE('',*,*,#8677,.T.);
#12407=ORIENTED_EDGE('',*,*,#8673,.T.);
#12408=ORIENTED_EDGE('',*,*,#8678,.F.);
#12409=ORIENTED_EDGE('',*,*,#8679,.F.);
#12410=ORIENTED_EDGE('',*,*,#8680,.T.);
#12411=ORIENTED_EDGE('',*,*,#8676,.T.);
#12412=ORIENTED_EDGE('',*,*,#8681,.F.);
#12413=ORIENTED_EDGE('',*,*,#8682,.F.);
#12414=ORIENTED_EDGE('',*,*,#8683,.T.);
#12415=ORIENTED_EDGE('',*,*,#8679,.T.);
#12416=ORIENTED_EDGE('',*,*,#8684,.F.);
#12417=ORIENTED_EDGE('',*,*,#8685,.F.);
#12418=ORIENTED_EDGE('',*,*,#8686,.T.);
#12419=ORIENTED_EDGE('',*,*,#8682,.T.);
#12420=ORIENTED_EDGE('',*,*,#8687,.F.);
#12421=ORIENTED_EDGE('',*,*,#8688,.F.);
#12422=ORIENTED_EDGE('',*,*,#8689,.T.);
#12423=ORIENTED_EDGE('',*,*,#8685,.T.);
#12424=ORIENTED_EDGE('',*,*,#8690,.F.);
#12425=ORIENTED_EDGE('',*,*,#8691,.F.);
#12426=ORIENTED_EDGE('',*,*,#8692,.T.);
#12427=ORIENTED_EDGE('',*,*,#8688,.T.);
#12428=ORIENTED_EDGE('',*,*,#8693,.F.);
#12429=ORIENTED_EDGE('',*,*,#8694,.F.);
#12430=ORIENTED_EDGE('',*,*,#8695,.T.);
#12431=ORIENTED_EDGE('',*,*,#8691,.T.);
#12432=ORIENTED_EDGE('',*,*,#8696,.F.);
#12433=ORIENTED_EDGE('',*,*,#8697,.F.);
#12434=ORIENTED_EDGE('',*,*,#8698,.T.);
#12435=ORIENTED_EDGE('',*,*,#8694,.T.);
#12436=ORIENTED_EDGE('',*,*,#8699,.F.);
#12437=ORIENTED_EDGE('',*,*,#8700,.F.);
#12438=ORIENTED_EDGE('',*,*,#8701,.T.);
#12439=ORIENTED_EDGE('',*,*,#8697,.T.);
#12440=ORIENTED_EDGE('',*,*,#8702,.F.);
#12441=ORIENTED_EDGE('',*,*,#8703,.F.);
#12442=ORIENTED_EDGE('',*,*,#8704,.T.);
#12443=ORIENTED_EDGE('',*,*,#8700,.T.);
#12444=ORIENTED_EDGE('',*,*,#8705,.F.);
#12445=ORIENTED_EDGE('',*,*,#8706,.F.);
#12446=ORIENTED_EDGE('',*,*,#8707,.T.);
#12447=ORIENTED_EDGE('',*,*,#8703,.T.);
#12448=ORIENTED_EDGE('',*,*,#8708,.F.);
#12449=ORIENTED_EDGE('',*,*,#8709,.F.);
#12450=ORIENTED_EDGE('',*,*,#8710,.T.);
#12451=ORIENTED_EDGE('',*,*,#8706,.T.);
#12452=ORIENTED_EDGE('',*,*,#8711,.F.);
#12453=ORIENTED_EDGE('',*,*,#8712,.F.);
#12454=ORIENTED_EDGE('',*,*,#8713,.T.);
#12455=ORIENTED_EDGE('',*,*,#8709,.T.);
#12456=ORIENTED_EDGE('',*,*,#8714,.F.);
#12457=ORIENTED_EDGE('',*,*,#8715,.F.);
#12458=ORIENTED_EDGE('',*,*,#8716,.T.);
#12459=ORIENTED_EDGE('',*,*,#8712,.T.);
#12460=ORIENTED_EDGE('',*,*,#8717,.F.);
#12461=ORIENTED_EDGE('',*,*,#8718,.F.);
#12462=ORIENTED_EDGE('',*,*,#8719,.T.);
#12463=ORIENTED_EDGE('',*,*,#8715,.T.);
#12464=ORIENTED_EDGE('',*,*,#8720,.F.);
#12465=ORIENTED_EDGE('',*,*,#8721,.F.);
#12466=ORIENTED_EDGE('',*,*,#8722,.F.);
#12467=ORIENTED_EDGE('',*,*,#8653,.F.);
#12468=ORIENTED_EDGE('',*,*,#8650,.F.);
#12469=ORIENTED_EDGE('',*,*,#8647,.F.);
#12470=ORIENTED_EDGE('',*,*,#8644,.F.);
#12471=ORIENTED_EDGE('',*,*,#8641,.F.);
#12472=ORIENTED_EDGE('',*,*,#8638,.F.);
#12473=ORIENTED_EDGE('',*,*,#8635,.F.);
#12474=ORIENTED_EDGE('',*,*,#8632,.F.);
#12475=ORIENTED_EDGE('',*,*,#8629,.F.);
#12476=ORIENTED_EDGE('',*,*,#8626,.F.);
#12477=ORIENTED_EDGE('',*,*,#8623,.F.);
#12478=ORIENTED_EDGE('',*,*,#8620,.F.);
#12479=ORIENTED_EDGE('',*,*,#8617,.F.);
#12480=ORIENTED_EDGE('',*,*,#8614,.F.);
#12481=ORIENTED_EDGE('',*,*,#8611,.F.);
#12482=ORIENTED_EDGE('',*,*,#8608,.F.);
#12483=ORIENTED_EDGE('',*,*,#8605,.F.);
#12484=ORIENTED_EDGE('',*,*,#8602,.F.);
#12485=ORIENTED_EDGE('',*,*,#8599,.F.);
#12486=ORIENTED_EDGE('',*,*,#8596,.F.);
#12487=ORIENTED_EDGE('',*,*,#8593,.F.);
#12488=ORIENTED_EDGE('',*,*,#8590,.F.);
#12489=ORIENTED_EDGE('',*,*,#8587,.F.);
#12490=ORIENTED_EDGE('',*,*,#8723,.F.);
#12491=ORIENTED_EDGE('',*,*,#8724,.T.);
#12492=ORIENTED_EDGE('',*,*,#8720,.T.);
#12493=ORIENTED_EDGE('',*,*,#8717,.T.);
#12494=ORIENTED_EDGE('',*,*,#8714,.T.);
#12495=ORIENTED_EDGE('',*,*,#8711,.T.);
#12496=ORIENTED_EDGE('',*,*,#8708,.T.);
#12497=ORIENTED_EDGE('',*,*,#8705,.T.);
#12498=ORIENTED_EDGE('',*,*,#8702,.T.);
#12499=ORIENTED_EDGE('',*,*,#8699,.T.);
#12500=ORIENTED_EDGE('',*,*,#8696,.T.);
#12501=ORIENTED_EDGE('',*,*,#8693,.T.);
#12502=ORIENTED_EDGE('',*,*,#8690,.T.);
#12503=ORIENTED_EDGE('',*,*,#8687,.T.);
#12504=ORIENTED_EDGE('',*,*,#8684,.T.);
#12505=ORIENTED_EDGE('',*,*,#8681,.T.);
#12506=ORIENTED_EDGE('',*,*,#8678,.T.);
#12507=ORIENTED_EDGE('',*,*,#8675,.T.);
#12508=ORIENTED_EDGE('',*,*,#8672,.T.);
#12509=ORIENTED_EDGE('',*,*,#8669,.T.);
#12510=ORIENTED_EDGE('',*,*,#8666,.T.);
#12511=ORIENTED_EDGE('',*,*,#8663,.T.);
#12512=ORIENTED_EDGE('',*,*,#8660,.T.);
#12513=ORIENTED_EDGE('',*,*,#8657,.T.);
#12514=ORIENTED_EDGE('',*,*,#8725,.T.);
#12515=ORIENTED_EDGE('',*,*,#8726,.T.);
#12516=ORIENTED_EDGE('',*,*,#8727,.T.);
#12517=ORIENTED_EDGE('',*,*,#8728,.T.);
#12518=ORIENTED_EDGE('',*,*,#8723,.T.);
#12519=ORIENTED_EDGE('',*,*,#8718,.T.);
#12520=ORIENTED_EDGE('',*,*,#8724,.F.);
#12521=ORIENTED_EDGE('',*,*,#8728,.F.);
#12522=ORIENTED_EDGE('',*,*,#8729,.T.);
#12523=ORIENTED_EDGE('',*,*,#8730,.F.);
#12524=ORIENTED_EDGE('',*,*,#8655,.F.);
#12525=ORIENTED_EDGE('',*,*,#8659,.F.);
#12526=ORIENTED_EDGE('',*,*,#8662,.F.);
#12527=ORIENTED_EDGE('',*,*,#8665,.F.);
#12528=ORIENTED_EDGE('',*,*,#8668,.F.);
#12529=ORIENTED_EDGE('',*,*,#8671,.F.);
#12530=ORIENTED_EDGE('',*,*,#8674,.F.);
#12531=ORIENTED_EDGE('',*,*,#8677,.F.);
#12532=ORIENTED_EDGE('',*,*,#8680,.F.);
#12533=ORIENTED_EDGE('',*,*,#8683,.F.);
#12534=ORIENTED_EDGE('',*,*,#8686,.F.);
#12535=ORIENTED_EDGE('',*,*,#8689,.F.);
#12536=ORIENTED_EDGE('',*,*,#8692,.F.);
#12537=ORIENTED_EDGE('',*,*,#8695,.F.);
#12538=ORIENTED_EDGE('',*,*,#8698,.F.);
#12539=ORIENTED_EDGE('',*,*,#8701,.F.);
#12540=ORIENTED_EDGE('',*,*,#8704,.F.);
#12541=ORIENTED_EDGE('',*,*,#8707,.F.);
#12542=ORIENTED_EDGE('',*,*,#8710,.F.);
#12543=ORIENTED_EDGE('',*,*,#8713,.F.);
#12544=ORIENTED_EDGE('',*,*,#8716,.F.);
#12545=ORIENTED_EDGE('',*,*,#8719,.F.);
#12546=ORIENTED_EDGE('',*,*,#8729,.F.);
#12547=ORIENTED_EDGE('',*,*,#8727,.F.);
#12548=ORIENTED_EDGE('',*,*,#8585,.F.);
#12549=ORIENTED_EDGE('',*,*,#8589,.F.);
#12550=ORIENTED_EDGE('',*,*,#8592,.F.);
#12551=ORIENTED_EDGE('',*,*,#8595,.F.);
#12552=ORIENTED_EDGE('',*,*,#8598,.F.);
#12553=ORIENTED_EDGE('',*,*,#8601,.F.);
#12554=ORIENTED_EDGE('',*,*,#8604,.F.);
#12555=ORIENTED_EDGE('',*,*,#8607,.F.);
#12556=ORIENTED_EDGE('',*,*,#8610,.F.);
#12557=ORIENTED_EDGE('',*,*,#8613,.F.);
#12558=ORIENTED_EDGE('',*,*,#8616,.F.);
#12559=ORIENTED_EDGE('',*,*,#8619,.F.);
#12560=ORIENTED_EDGE('',*,*,#8622,.F.);
#12561=ORIENTED_EDGE('',*,*,#8625,.F.);
#12562=ORIENTED_EDGE('',*,*,#8628,.F.);
#12563=ORIENTED_EDGE('',*,*,#8631,.F.);
#12564=ORIENTED_EDGE('',*,*,#8634,.F.);
#12565=ORIENTED_EDGE('',*,*,#8637,.F.);
#12566=ORIENTED_EDGE('',*,*,#8640,.F.);
#12567=ORIENTED_EDGE('',*,*,#8643,.F.);
#12568=ORIENTED_EDGE('',*,*,#8646,.F.);
#12569=ORIENTED_EDGE('',*,*,#8649,.F.);
#12570=ORIENTED_EDGE('',*,*,#8652,.F.);
#12571=ORIENTED_EDGE('',*,*,#8731,.F.);
#12572=ORIENTED_EDGE('',*,*,#8651,.T.);
#12573=ORIENTED_EDGE('',*,*,#8722,.T.);
#12574=ORIENTED_EDGE('',*,*,#8732,.F.);
#12575=ORIENTED_EDGE('',*,*,#8731,.T.);
#12576=ORIENTED_EDGE('',*,*,#8733,.F.);
#12577=ORIENTED_EDGE('',*,*,#8725,.F.);
#12578=ORIENTED_EDGE('',*,*,#8586,.F.);
#12579=ORIENTED_EDGE('',*,*,#8726,.F.);
#12580=ORIENTED_EDGE('',*,*,#8734,.T.);
#12581=ORIENTED_EDGE('',*,*,#8733,.T.);
#12582=ORIENTED_EDGE('',*,*,#8734,.F.);
#12583=ORIENTED_EDGE('',*,*,#8735,.F.);
#12584=ORIENTED_EDGE('',*,*,#8736,.F.);
#12585=ORIENTED_EDGE('',*,*,#8737,.F.);
#12586=ORIENTED_EDGE('',*,*,#8738,.F.);
#12587=ORIENTED_EDGE('',*,*,#8739,.F.);
#12588=ORIENTED_EDGE('',*,*,#8740,.T.);
#12589=ORIENTED_EDGE('',*,*,#8741,.F.);
#12590=ORIENTED_EDGE('',*,*,#8740,.F.);
#12591=ORIENTED_EDGE('',*,*,#8742,.F.);
#12592=ORIENTED_EDGE('',*,*,#8743,.F.);
#12593=ORIENTED_EDGE('',*,*,#8738,.T.);
#12594=ORIENTED_EDGE('',*,*,#8744,.F.);
#12595=ORIENTED_EDGE('',*,*,#8745,.T.);
#12596=ORIENTED_EDGE('',*,*,#8746,.T.);
#12597=ORIENTED_EDGE('',*,*,#8737,.T.);
#12598=ORIENTED_EDGE('',*,*,#8747,.F.);
#12599=ORIENTED_EDGE('',*,*,#8748,.T.);
#12600=ORIENTED_EDGE('',*,*,#8744,.T.);
#12601=ORIENTED_EDGE('',*,*,#8736,.T.);
#12602=ORIENTED_EDGE('',*,*,#8749,.F.);
#12603=ORIENTED_EDGE('',*,*,#8750,.T.);
#12604=ORIENTED_EDGE('',*,*,#8747,.T.);
#12605=ORIENTED_EDGE('',*,*,#8735,.T.);
#12606=ORIENTED_EDGE('',*,*,#8751,.F.);
#12607=ORIENTED_EDGE('',*,*,#8752,.T.);
#12608=ORIENTED_EDGE('',*,*,#8749,.T.);
#12609=ORIENTED_EDGE('',*,*,#8743,.T.);
#12610=ORIENTED_EDGE('',*,*,#8753,.F.);
#12611=ORIENTED_EDGE('',*,*,#8754,.T.);
#12612=ORIENTED_EDGE('',*,*,#8751,.T.);
#12613=ORIENTED_EDGE('',*,*,#8742,.T.);
#12614=ORIENTED_EDGE('',*,*,#8739,.T.);
#12615=ORIENTED_EDGE('',*,*,#8746,.F.);
#12616=ORIENTED_EDGE('',*,*,#8755,.T.);
#12617=ORIENTED_EDGE('',*,*,#8753,.T.);
#12618=ORIENTED_EDGE('',*,*,#8741,.T.);
#12619=ORIENTED_EDGE('',*,*,#8750,.F.);
#12620=ORIENTED_EDGE('',*,*,#8752,.F.);
#12621=ORIENTED_EDGE('',*,*,#8754,.F.);
#12622=ORIENTED_EDGE('',*,*,#8755,.F.);
#12623=ORIENTED_EDGE('',*,*,#8745,.F.);
#12624=ORIENTED_EDGE('',*,*,#8748,.F.);
#12625=ORIENTED_EDGE('',*,*,#8732,.T.);
#12626=ORIENTED_EDGE('',*,*,#8721,.T.);
#12627=ORIENTED_EDGE('',*,*,#8656,.T.);
#12628=ORIENTED_EDGE('',*,*,#8730,.T.);
#12629=ORIENTED_EDGE('',*,*,#8756,.F.);
#12630=ORIENTED_EDGE('',*,*,#8757,.T.);
#12631=ORIENTED_EDGE('',*,*,#8758,.T.);
#12632=ORIENTED_EDGE('',*,*,#8759,.T.);
#12633=ORIENTED_EDGE('',*,*,#8760,.F.);
#12634=ORIENTED_EDGE('',*,*,#8761,.T.);
#12635=ORIENTED_EDGE('',*,*,#8756,.T.);
#12636=ORIENTED_EDGE('',*,*,#8762,.T.);
#12637=ORIENTED_EDGE('',*,*,#8763,.F.);
#12638=ORIENTED_EDGE('',*,*,#8764,.T.);
#12639=ORIENTED_EDGE('',*,*,#8760,.T.);
#12640=ORIENTED_EDGE('',*,*,#8765,.T.);
#12641=ORIENTED_EDGE('',*,*,#8766,.F.);
#12642=ORIENTED_EDGE('',*,*,#8767,.T.);
#12643=ORIENTED_EDGE('',*,*,#8763,.T.);
#12644=ORIENTED_EDGE('',*,*,#8768,.T.);
#12645=ORIENTED_EDGE('',*,*,#8769,.F.);
#12646=ORIENTED_EDGE('',*,*,#8770,.T.);
#12647=ORIENTED_EDGE('',*,*,#8766,.T.);
#12648=ORIENTED_EDGE('',*,*,#8771,.T.);
#12649=ORIENTED_EDGE('',*,*,#8772,.F.);
#12650=ORIENTED_EDGE('',*,*,#8773,.T.);
#12651=ORIENTED_EDGE('',*,*,#8769,.T.);
#12652=ORIENTED_EDGE('',*,*,#8774,.T.);
#12653=ORIENTED_EDGE('',*,*,#8775,.F.);
#12654=ORIENTED_EDGE('',*,*,#8776,.T.);
#12655=ORIENTED_EDGE('',*,*,#8772,.T.);
#12656=ORIENTED_EDGE('',*,*,#8777,.T.);
#12657=ORIENTED_EDGE('',*,*,#8778,.F.);
#12658=ORIENTED_EDGE('',*,*,#8779,.T.);
#12659=ORIENTED_EDGE('',*,*,#8775,.T.);
#12660=ORIENTED_EDGE('',*,*,#8780,.T.);
#12661=ORIENTED_EDGE('',*,*,#8781,.F.);
#12662=ORIENTED_EDGE('',*,*,#8782,.T.);
#12663=ORIENTED_EDGE('',*,*,#8778,.T.);
#12664=ORIENTED_EDGE('',*,*,#8783,.T.);
#12665=ORIENTED_EDGE('',*,*,#8784,.F.);
#12666=ORIENTED_EDGE('',*,*,#8785,.T.);
#12667=ORIENTED_EDGE('',*,*,#8781,.T.);
#12668=ORIENTED_EDGE('',*,*,#8786,.T.);
#12669=ORIENTED_EDGE('',*,*,#8787,.F.);
#12670=ORIENTED_EDGE('',*,*,#8788,.T.);
#12671=ORIENTED_EDGE('',*,*,#8784,.T.);
#12672=ORIENTED_EDGE('',*,*,#8789,.T.);
#12673=ORIENTED_EDGE('',*,*,#8790,.F.);
#12674=ORIENTED_EDGE('',*,*,#8791,.T.);
#12675=ORIENTED_EDGE('',*,*,#8787,.T.);
#12676=ORIENTED_EDGE('',*,*,#8792,.T.);
#12677=ORIENTED_EDGE('',*,*,#8793,.F.);
#12678=ORIENTED_EDGE('',*,*,#8794,.T.);
#12679=ORIENTED_EDGE('',*,*,#8790,.T.);
#12680=ORIENTED_EDGE('',*,*,#8795,.T.);
#12681=ORIENTED_EDGE('',*,*,#8796,.F.);
#12682=ORIENTED_EDGE('',*,*,#8797,.T.);
#12683=ORIENTED_EDGE('',*,*,#8793,.T.);
#12684=ORIENTED_EDGE('',*,*,#8798,.T.);
#12685=ORIENTED_EDGE('',*,*,#8799,.F.);
#12686=ORIENTED_EDGE('',*,*,#8800,.T.);
#12687=ORIENTED_EDGE('',*,*,#8796,.T.);
#12688=ORIENTED_EDGE('',*,*,#8801,.T.);
#12689=ORIENTED_EDGE('',*,*,#8802,.F.);
#12690=ORIENTED_EDGE('',*,*,#8803,.T.);
#12691=ORIENTED_EDGE('',*,*,#8799,.T.);
#12692=ORIENTED_EDGE('',*,*,#8804,.T.);
#12693=ORIENTED_EDGE('',*,*,#8805,.F.);
#12694=ORIENTED_EDGE('',*,*,#8806,.T.);
#12695=ORIENTED_EDGE('',*,*,#8802,.T.);
#12696=ORIENTED_EDGE('',*,*,#8807,.T.);
#12697=ORIENTED_EDGE('',*,*,#8808,.F.);
#12698=ORIENTED_EDGE('',*,*,#8809,.T.);
#12699=ORIENTED_EDGE('',*,*,#8805,.T.);
#12700=ORIENTED_EDGE('',*,*,#8810,.T.);
#12701=ORIENTED_EDGE('',*,*,#8811,.F.);
#12702=ORIENTED_EDGE('',*,*,#8812,.T.);
#12703=ORIENTED_EDGE('',*,*,#8808,.T.);
#12704=ORIENTED_EDGE('',*,*,#8813,.T.);
#12705=ORIENTED_EDGE('',*,*,#8814,.F.);
#12706=ORIENTED_EDGE('',*,*,#8815,.T.);
#12707=ORIENTED_EDGE('',*,*,#8811,.T.);
#12708=ORIENTED_EDGE('',*,*,#8816,.T.);
#12709=ORIENTED_EDGE('',*,*,#8817,.F.);
#12710=ORIENTED_EDGE('',*,*,#8818,.T.);
#12711=ORIENTED_EDGE('',*,*,#8814,.T.);
#12712=ORIENTED_EDGE('',*,*,#8819,.T.);
#12713=ORIENTED_EDGE('',*,*,#8820,.F.);
#12714=ORIENTED_EDGE('',*,*,#8821,.T.);
#12715=ORIENTED_EDGE('',*,*,#8817,.T.);
#12716=ORIENTED_EDGE('',*,*,#8822,.T.);
#12717=ORIENTED_EDGE('',*,*,#8823,.F.);
#12718=ORIENTED_EDGE('',*,*,#8824,.T.);
#12719=ORIENTED_EDGE('',*,*,#8820,.T.);
#12720=ORIENTED_EDGE('',*,*,#8825,.T.);
#12721=ORIENTED_EDGE('',*,*,#8826,.F.);
#12722=ORIENTED_EDGE('',*,*,#8827,.T.);
#12723=ORIENTED_EDGE('',*,*,#8823,.T.);
#12724=ORIENTED_EDGE('',*,*,#8828,.T.);
#12725=ORIENTED_EDGE('',*,*,#8829,.F.);
#12726=ORIENTED_EDGE('',*,*,#8830,.T.);
#12727=ORIENTED_EDGE('',*,*,#8826,.T.);
#12728=ORIENTED_EDGE('',*,*,#8831,.T.);
#12729=ORIENTED_EDGE('',*,*,#8832,.F.);
#12730=ORIENTED_EDGE('',*,*,#8833,.T.);
#12731=ORIENTED_EDGE('',*,*,#8829,.T.);
#12732=ORIENTED_EDGE('',*,*,#8834,.T.);
#12733=ORIENTED_EDGE('',*,*,#8835,.F.);
#12734=ORIENTED_EDGE('',*,*,#8836,.T.);
#12735=ORIENTED_EDGE('',*,*,#8832,.T.);
#12736=ORIENTED_EDGE('',*,*,#8837,.T.);
#12737=ORIENTED_EDGE('',*,*,#8838,.F.);
#12738=ORIENTED_EDGE('',*,*,#8839,.T.);
#12739=ORIENTED_EDGE('',*,*,#8835,.T.);
#12740=ORIENTED_EDGE('',*,*,#8840,.T.);
#12741=ORIENTED_EDGE('',*,*,#8841,.F.);
#12742=ORIENTED_EDGE('',*,*,#8842,.T.);
#12743=ORIENTED_EDGE('',*,*,#8843,.F.);
#12744=ORIENTED_EDGE('',*,*,#8844,.F.);
#12745=ORIENTED_EDGE('',*,*,#8845,.F.);
#12746=ORIENTED_EDGE('',*,*,#8846,.T.);
#12747=ORIENTED_EDGE('',*,*,#8841,.T.);
#12748=ORIENTED_EDGE('',*,*,#8847,.F.);
#12749=ORIENTED_EDGE('',*,*,#8848,.F.);
#12750=ORIENTED_EDGE('',*,*,#8849,.T.);
#12751=ORIENTED_EDGE('',*,*,#8845,.T.);
#12752=ORIENTED_EDGE('',*,*,#8850,.F.);
#12753=ORIENTED_EDGE('',*,*,#8851,.F.);
#12754=ORIENTED_EDGE('',*,*,#8852,.T.);
#12755=ORIENTED_EDGE('',*,*,#8848,.T.);
#12756=ORIENTED_EDGE('',*,*,#8853,.F.);
#12757=ORIENTED_EDGE('',*,*,#8854,.F.);
#12758=ORIENTED_EDGE('',*,*,#8855,.T.);
#12759=ORIENTED_EDGE('',*,*,#8851,.T.);
#12760=ORIENTED_EDGE('',*,*,#8856,.F.);
#12761=ORIENTED_EDGE('',*,*,#8857,.F.);
#12762=ORIENTED_EDGE('',*,*,#8858,.T.);
#12763=ORIENTED_EDGE('',*,*,#8854,.T.);
#12764=ORIENTED_EDGE('',*,*,#8859,.F.);
#12765=ORIENTED_EDGE('',*,*,#8860,.F.);
#12766=ORIENTED_EDGE('',*,*,#8861,.T.);
#12767=ORIENTED_EDGE('',*,*,#8857,.T.);
#12768=ORIENTED_EDGE('',*,*,#8862,.F.);
#12769=ORIENTED_EDGE('',*,*,#8863,.F.);
#12770=ORIENTED_EDGE('',*,*,#8864,.T.);
#12771=ORIENTED_EDGE('',*,*,#8860,.T.);
#12772=ORIENTED_EDGE('',*,*,#8865,.F.);
#12773=ORIENTED_EDGE('',*,*,#8866,.F.);
#12774=ORIENTED_EDGE('',*,*,#8867,.T.);
#12775=ORIENTED_EDGE('',*,*,#8863,.T.);
#12776=ORIENTED_EDGE('',*,*,#8868,.F.);
#12777=ORIENTED_EDGE('',*,*,#8869,.F.);
#12778=ORIENTED_EDGE('',*,*,#8870,.T.);
#12779=ORIENTED_EDGE('',*,*,#8866,.T.);
#12780=ORIENTED_EDGE('',*,*,#8871,.F.);
#12781=ORIENTED_EDGE('',*,*,#8872,.F.);
#12782=ORIENTED_EDGE('',*,*,#8873,.T.);
#12783=ORIENTED_EDGE('',*,*,#8869,.T.);
#12784=ORIENTED_EDGE('',*,*,#8874,.F.);
#12785=ORIENTED_EDGE('',*,*,#8875,.F.);
#12786=ORIENTED_EDGE('',*,*,#8876,.T.);
#12787=ORIENTED_EDGE('',*,*,#8872,.T.);
#12788=ORIENTED_EDGE('',*,*,#8877,.F.);
#12789=ORIENTED_EDGE('',*,*,#8878,.F.);
#12790=ORIENTED_EDGE('',*,*,#8879,.T.);
#12791=ORIENTED_EDGE('',*,*,#8875,.T.);
#12792=ORIENTED_EDGE('',*,*,#8880,.F.);
#12793=ORIENTED_EDGE('',*,*,#8881,.F.);
#12794=ORIENTED_EDGE('',*,*,#8882,.T.);
#12795=ORIENTED_EDGE('',*,*,#8878,.T.);
#12796=ORIENTED_EDGE('',*,*,#8883,.F.);
#12797=ORIENTED_EDGE('',*,*,#8884,.F.);
#12798=ORIENTED_EDGE('',*,*,#8885,.T.);
#12799=ORIENTED_EDGE('',*,*,#8881,.T.);
#12800=ORIENTED_EDGE('',*,*,#8886,.F.);
#12801=ORIENTED_EDGE('',*,*,#8887,.F.);
#12802=ORIENTED_EDGE('',*,*,#8888,.T.);
#12803=ORIENTED_EDGE('',*,*,#8884,.T.);
#12804=ORIENTED_EDGE('',*,*,#8889,.F.);
#12805=ORIENTED_EDGE('',*,*,#8890,.F.);
#12806=ORIENTED_EDGE('',*,*,#8891,.T.);
#12807=ORIENTED_EDGE('',*,*,#8887,.T.);
#12808=ORIENTED_EDGE('',*,*,#8892,.F.);
#12809=ORIENTED_EDGE('',*,*,#8893,.F.);
#12810=ORIENTED_EDGE('',*,*,#8894,.T.);
#12811=ORIENTED_EDGE('',*,*,#8890,.T.);
#12812=ORIENTED_EDGE('',*,*,#8895,.F.);
#12813=ORIENTED_EDGE('',*,*,#8896,.F.);
#12814=ORIENTED_EDGE('',*,*,#8897,.T.);
#12815=ORIENTED_EDGE('',*,*,#8893,.T.);
#12816=ORIENTED_EDGE('',*,*,#8898,.F.);
#12817=ORIENTED_EDGE('',*,*,#8899,.F.);
#12818=ORIENTED_EDGE('',*,*,#8900,.T.);
#12819=ORIENTED_EDGE('',*,*,#8896,.T.);
#12820=ORIENTED_EDGE('',*,*,#8901,.F.);
#12821=ORIENTED_EDGE('',*,*,#8902,.F.);
#12822=ORIENTED_EDGE('',*,*,#8903,.T.);
#12823=ORIENTED_EDGE('',*,*,#8899,.T.);
#12824=ORIENTED_EDGE('',*,*,#8904,.F.);
#12825=ORIENTED_EDGE('',*,*,#8905,.F.);
#12826=ORIENTED_EDGE('',*,*,#8906,.T.);
#12827=ORIENTED_EDGE('',*,*,#8902,.T.);
#12828=ORIENTED_EDGE('',*,*,#8907,.F.);
#12829=ORIENTED_EDGE('',*,*,#8908,.F.);
#12830=ORIENTED_EDGE('',*,*,#8909,.T.);
#12831=ORIENTED_EDGE('',*,*,#8905,.T.);
#12832=ORIENTED_EDGE('',*,*,#8910,.F.);
#12833=ORIENTED_EDGE('',*,*,#8911,.F.);
#12834=ORIENTED_EDGE('',*,*,#8912,.T.);
#12835=ORIENTED_EDGE('',*,*,#8908,.T.);
#12836=ORIENTED_EDGE('',*,*,#8913,.F.);
#12837=ORIENTED_EDGE('',*,*,#8914,.F.);
#12838=ORIENTED_EDGE('',*,*,#8915,.T.);
#12839=ORIENTED_EDGE('',*,*,#8911,.T.);
#12840=ORIENTED_EDGE('',*,*,#8916,.F.);
#12841=ORIENTED_EDGE('',*,*,#8917,.F.);
#12842=ORIENTED_EDGE('',*,*,#8918,.T.);
#12843=ORIENTED_EDGE('',*,*,#8914,.T.);
#12844=ORIENTED_EDGE('',*,*,#8919,.F.);
#12845=ORIENTED_EDGE('',*,*,#8920,.F.);
#12846=ORIENTED_EDGE('',*,*,#8921,.T.);
#12847=ORIENTED_EDGE('',*,*,#8917,.T.);
#12848=ORIENTED_EDGE('',*,*,#8922,.F.);
#12849=ORIENTED_EDGE('',*,*,#8923,.F.);
#12850=ORIENTED_EDGE('',*,*,#8924,.T.);
#12851=ORIENTED_EDGE('',*,*,#8920,.T.);
#12852=ORIENTED_EDGE('',*,*,#8925,.F.);
#12853=ORIENTED_EDGE('',*,*,#8926,.F.);
#12854=ORIENTED_EDGE('',*,*,#8927,.F.);
#12855=ORIENTED_EDGE('',*,*,#8840,.F.);
#12856=ORIENTED_EDGE('',*,*,#8837,.F.);
#12857=ORIENTED_EDGE('',*,*,#8834,.F.);
#12858=ORIENTED_EDGE('',*,*,#8831,.F.);
#12859=ORIENTED_EDGE('',*,*,#8828,.F.);
#12860=ORIENTED_EDGE('',*,*,#8825,.F.);
#12861=ORIENTED_EDGE('',*,*,#8822,.F.);
#12862=ORIENTED_EDGE('',*,*,#8819,.F.);
#12863=ORIENTED_EDGE('',*,*,#8816,.F.);
#12864=ORIENTED_EDGE('',*,*,#8813,.F.);
#12865=ORIENTED_EDGE('',*,*,#8810,.F.);
#12866=ORIENTED_EDGE('',*,*,#8807,.F.);
#12867=ORIENTED_EDGE('',*,*,#8804,.F.);
#12868=ORIENTED_EDGE('',*,*,#8801,.F.);
#12869=ORIENTED_EDGE('',*,*,#8798,.F.);
#12870=ORIENTED_EDGE('',*,*,#8795,.F.);
#12871=ORIENTED_EDGE('',*,*,#8792,.F.);
#12872=ORIENTED_EDGE('',*,*,#8789,.F.);
#12873=ORIENTED_EDGE('',*,*,#8786,.F.);
#12874=ORIENTED_EDGE('',*,*,#8783,.F.);
#12875=ORIENTED_EDGE('',*,*,#8780,.F.);
#12876=ORIENTED_EDGE('',*,*,#8777,.F.);
#12877=ORIENTED_EDGE('',*,*,#8774,.F.);
#12878=ORIENTED_EDGE('',*,*,#8771,.F.);
#12879=ORIENTED_EDGE('',*,*,#8768,.F.);
#12880=ORIENTED_EDGE('',*,*,#8765,.F.);
#12881=ORIENTED_EDGE('',*,*,#8762,.F.);
#12882=ORIENTED_EDGE('',*,*,#8759,.F.);
#12883=ORIENTED_EDGE('',*,*,#8928,.F.);
#12884=ORIENTED_EDGE('',*,*,#8929,.T.);
#12885=ORIENTED_EDGE('',*,*,#8925,.T.);
#12886=ORIENTED_EDGE('',*,*,#8922,.T.);
#12887=ORIENTED_EDGE('',*,*,#8919,.T.);
#12888=ORIENTED_EDGE('',*,*,#8916,.T.);
#12889=ORIENTED_EDGE('',*,*,#8913,.T.);
#12890=ORIENTED_EDGE('',*,*,#8910,.T.);
#12891=ORIENTED_EDGE('',*,*,#8907,.T.);
#12892=ORIENTED_EDGE('',*,*,#8904,.T.);
#12893=ORIENTED_EDGE('',*,*,#8901,.T.);
#12894=ORIENTED_EDGE('',*,*,#8898,.T.);
#12895=ORIENTED_EDGE('',*,*,#8895,.T.);
#12896=ORIENTED_EDGE('',*,*,#8892,.T.);
#12897=ORIENTED_EDGE('',*,*,#8889,.T.);
#12898=ORIENTED_EDGE('',*,*,#8886,.T.);
#12899=ORIENTED_EDGE('',*,*,#8883,.T.);
#12900=ORIENTED_EDGE('',*,*,#8880,.T.);
#12901=ORIENTED_EDGE('',*,*,#8877,.T.);
#12902=ORIENTED_EDGE('',*,*,#8874,.T.);
#12903=ORIENTED_EDGE('',*,*,#8871,.T.);
#12904=ORIENTED_EDGE('',*,*,#8868,.T.);
#12905=ORIENTED_EDGE('',*,*,#8865,.T.);
#12906=ORIENTED_EDGE('',*,*,#8862,.T.);
#12907=ORIENTED_EDGE('',*,*,#8859,.T.);
#12908=ORIENTED_EDGE('',*,*,#8856,.T.);
#12909=ORIENTED_EDGE('',*,*,#8853,.T.);
#12910=ORIENTED_EDGE('',*,*,#8850,.T.);
#12911=ORIENTED_EDGE('',*,*,#8847,.T.);
#12912=ORIENTED_EDGE('',*,*,#8844,.T.);
#12913=ORIENTED_EDGE('',*,*,#8930,.T.);
#12914=ORIENTED_EDGE('',*,*,#8931,.T.);
#12915=ORIENTED_EDGE('',*,*,#8932,.T.);
#12916=ORIENTED_EDGE('',*,*,#8933,.T.);
#12917=ORIENTED_EDGE('',*,*,#8928,.T.);
#12918=ORIENTED_EDGE('',*,*,#8923,.T.);
#12919=ORIENTED_EDGE('',*,*,#8929,.F.);
#12920=ORIENTED_EDGE('',*,*,#8933,.F.);
#12921=ORIENTED_EDGE('',*,*,#8934,.T.);
#12922=ORIENTED_EDGE('',*,*,#8935,.F.);
#12923=ORIENTED_EDGE('',*,*,#8842,.F.);
#12924=ORIENTED_EDGE('',*,*,#8846,.F.);
#12925=ORIENTED_EDGE('',*,*,#8849,.F.);
#12926=ORIENTED_EDGE('',*,*,#8852,.F.);
#12927=ORIENTED_EDGE('',*,*,#8855,.F.);
#12928=ORIENTED_EDGE('',*,*,#8858,.F.);
#12929=ORIENTED_EDGE('',*,*,#8861,.F.);
#12930=ORIENTED_EDGE('',*,*,#8864,.F.);
#12931=ORIENTED_EDGE('',*,*,#8867,.F.);
#12932=ORIENTED_EDGE('',*,*,#8870,.F.);
#12933=ORIENTED_EDGE('',*,*,#8873,.F.);
#12934=ORIENTED_EDGE('',*,*,#8876,.F.);
#12935=ORIENTED_EDGE('',*,*,#8879,.F.);
#12936=ORIENTED_EDGE('',*,*,#8882,.F.);
#12937=ORIENTED_EDGE('',*,*,#8885,.F.);
#12938=ORIENTED_EDGE('',*,*,#8888,.F.);
#12939=ORIENTED_EDGE('',*,*,#8891,.F.);
#12940=ORIENTED_EDGE('',*,*,#8894,.F.);
#12941=ORIENTED_EDGE('',*,*,#8897,.F.);
#12942=ORIENTED_EDGE('',*,*,#8900,.F.);
#12943=ORIENTED_EDGE('',*,*,#8903,.F.);
#12944=ORIENTED_EDGE('',*,*,#8906,.F.);
#12945=ORIENTED_EDGE('',*,*,#8909,.F.);
#12946=ORIENTED_EDGE('',*,*,#8912,.F.);
#12947=ORIENTED_EDGE('',*,*,#8915,.F.);
#12948=ORIENTED_EDGE('',*,*,#8918,.F.);
#12949=ORIENTED_EDGE('',*,*,#8921,.F.);
#12950=ORIENTED_EDGE('',*,*,#8924,.F.);
#12951=ORIENTED_EDGE('',*,*,#8934,.F.);
#12952=ORIENTED_EDGE('',*,*,#8932,.F.);
#12953=ORIENTED_EDGE('',*,*,#8757,.F.);
#12954=ORIENTED_EDGE('',*,*,#8761,.F.);
#12955=ORIENTED_EDGE('',*,*,#8764,.F.);
#12956=ORIENTED_EDGE('',*,*,#8767,.F.);
#12957=ORIENTED_EDGE('',*,*,#8770,.F.);
#12958=ORIENTED_EDGE('',*,*,#8773,.F.);
#12959=ORIENTED_EDGE('',*,*,#8776,.F.);
#12960=ORIENTED_EDGE('',*,*,#8779,.F.);
#12961=ORIENTED_EDGE('',*,*,#8782,.F.);
#12962=ORIENTED_EDGE('',*,*,#8785,.F.);
#12963=ORIENTED_EDGE('',*,*,#8788,.F.);
#12964=ORIENTED_EDGE('',*,*,#8791,.F.);
#12965=ORIENTED_EDGE('',*,*,#8794,.F.);
#12966=ORIENTED_EDGE('',*,*,#8797,.F.);
#12967=ORIENTED_EDGE('',*,*,#8800,.F.);
#12968=ORIENTED_EDGE('',*,*,#8803,.F.);
#12969=ORIENTED_EDGE('',*,*,#8806,.F.);
#12970=ORIENTED_EDGE('',*,*,#8809,.F.);
#12971=ORIENTED_EDGE('',*,*,#8812,.F.);
#12972=ORIENTED_EDGE('',*,*,#8815,.F.);
#12973=ORIENTED_EDGE('',*,*,#8818,.F.);
#12974=ORIENTED_EDGE('',*,*,#8821,.F.);
#12975=ORIENTED_EDGE('',*,*,#8824,.F.);
#12976=ORIENTED_EDGE('',*,*,#8827,.F.);
#12977=ORIENTED_EDGE('',*,*,#8830,.F.);
#12978=ORIENTED_EDGE('',*,*,#8833,.F.);
#12979=ORIENTED_EDGE('',*,*,#8836,.F.);
#12980=ORIENTED_EDGE('',*,*,#8839,.F.);
#12981=ORIENTED_EDGE('',*,*,#8936,.F.);
#12982=ORIENTED_EDGE('',*,*,#8937,.T.);
#12983=ORIENTED_EDGE('',*,*,#8938,.F.);
#12984=ORIENTED_EDGE('',*,*,#8937,.F.);
#12985=ORIENTED_EDGE('',*,*,#8939,.F.);
#12986=ORIENTED_EDGE('',*,*,#8940,.T.);
#12987=ORIENTED_EDGE('',*,*,#8941,.T.);
#12988=ORIENTED_EDGE('',*,*,#8942,.F.);
#12989=ORIENTED_EDGE('',*,*,#8943,.F.);
#12990=ORIENTED_EDGE('',*,*,#8942,.T.);
#12991=ORIENTED_EDGE('',*,*,#8944,.T.);
#12992=ORIENTED_EDGE('',*,*,#8945,.F.);
#12993=ORIENTED_EDGE('',*,*,#8946,.F.);
#12994=ORIENTED_EDGE('',*,*,#8945,.T.);
#12995=ORIENTED_EDGE('',*,*,#8947,.T.);
#12996=ORIENTED_EDGE('',*,*,#8948,.F.);
#12997=ORIENTED_EDGE('',*,*,#8949,.F.);
#12998=ORIENTED_EDGE('',*,*,#8948,.T.);
#12999=ORIENTED_EDGE('',*,*,#8950,.T.);
#13000=ORIENTED_EDGE('',*,*,#8951,.F.);
#13001=ORIENTED_EDGE('',*,*,#8952,.F.);
#13002=ORIENTED_EDGE('',*,*,#8953,.T.);
#13003=ORIENTED_EDGE('',*,*,#8954,.T.);
#13004=ORIENTED_EDGE('',*,*,#8940,.F.);
#13005=ORIENTED_EDGE('',*,*,#8955,.F.);
#13006=ORIENTED_EDGE('',*,*,#8951,.T.);
#13007=ORIENTED_EDGE('',*,*,#8956,.T.);
#13008=ORIENTED_EDGE('',*,*,#8953,.F.);
#13009=ORIENTED_EDGE('',*,*,#8956,.F.);
#13010=ORIENTED_EDGE('',*,*,#8950,.F.);
#13011=ORIENTED_EDGE('',*,*,#8947,.F.);
#13012=ORIENTED_EDGE('',*,*,#8944,.F.);
#13013=ORIENTED_EDGE('',*,*,#8941,.F.);
#13014=ORIENTED_EDGE('',*,*,#8954,.F.);
#13015=ORIENTED_EDGE('',*,*,#8938,.T.);
#13016=ORIENTED_EDGE('',*,*,#8957,.F.);
#13017=ORIENTED_EDGE('',*,*,#8930,.F.);
#13018=ORIENTED_EDGE('',*,*,#8758,.F.);
#13019=ORIENTED_EDGE('',*,*,#8931,.F.);
#13020=ORIENTED_EDGE('',*,*,#8958,.T.);
#13021=ORIENTED_EDGE('',*,*,#8957,.T.);
#13022=ORIENTED_EDGE('',*,*,#8958,.F.);
#13023=ORIENTED_EDGE('',*,*,#8838,.T.);
#13024=ORIENTED_EDGE('',*,*,#8927,.T.);
#13025=ORIENTED_EDGE('',*,*,#8959,.F.);
#13026=ORIENTED_EDGE('',*,*,#8936,.T.);
#13027=ORIENTED_EDGE('',*,*,#8960,.F.);
#13028=ORIENTED_EDGE('',*,*,#8959,.T.);
#13029=ORIENTED_EDGE('',*,*,#8926,.T.);
#13030=ORIENTED_EDGE('',*,*,#8843,.T.);
#13031=ORIENTED_EDGE('',*,*,#8935,.T.);
#13032=ORIENTED_EDGE('',*,*,#8961,.F.);
#13033=ORIENTED_EDGE('',*,*,#8962,.T.);
#13034=ORIENTED_EDGE('',*,*,#8960,.T.);
#13035=ORIENTED_EDGE('',*,*,#8962,.F.);
#13036=ORIENTED_EDGE('',*,*,#8963,.F.);
#13037=ORIENTED_EDGE('',*,*,#8949,.T.);
#13038=ORIENTED_EDGE('',*,*,#8955,.T.);
#13039=ORIENTED_EDGE('',*,*,#8952,.T.);
#13040=ORIENTED_EDGE('',*,*,#8939,.T.);
#13041=ORIENTED_EDGE('',*,*,#8943,.T.);
#13042=ORIENTED_EDGE('',*,*,#8946,.T.);
#13043=ORIENTED_EDGE('',*,*,#8964,.T.);
#13044=ORIENTED_EDGE('',*,*,#8963,.T.);
#13045=ORIENTED_EDGE('',*,*,#8961,.T.);
#13046=ORIENTED_EDGE('',*,*,#8964,.F.);
#13047=ORIENTED_EDGE('',*,*,#8965,.T.);
#13048=ORIENTED_EDGE('',*,*,#8966,.T.);
#13049=ORIENTED_EDGE('',*,*,#8967,.T.);
#13050=ORIENTED_EDGE('',*,*,#8968,.T.);
#13051=ORIENTED_EDGE('',*,*,#8966,.F.);
#13052=ORIENTED_EDGE('',*,*,#8967,.F.);
#13053=ORIENTED_EDGE('',*,*,#8968,.F.);
#13054=ORIENTED_EDGE('',*,*,#8969,.T.);
#13055=ORIENTED_EDGE('',*,*,#8970,.T.);
#13056=ORIENTED_EDGE('',*,*,#8969,.F.);
#13057=ORIENTED_EDGE('',*,*,#8965,.F.);
#13058=ORIENTED_EDGE('',*,*,#8971,.F.);
#13059=ORIENTED_EDGE('',*,*,#8971,.T.);
#13060=ORIENTED_EDGE('',*,*,#8972,.T.);
#13061=ORIENTED_EDGE('',*,*,#8973,.F.);
#13062=ORIENTED_EDGE('',*,*,#8972,.F.);
#13063=ORIENTED_EDGE('',*,*,#8974,.F.);
#13064=ORIENTED_EDGE('',*,*,#8973,.T.);
#13065=ORIENTED_EDGE('',*,*,#8970,.F.);
#13066=ORIENTED_EDGE('',*,*,#8975,.T.);
#13067=ORIENTED_EDGE('',*,*,#8974,.T.);
#13068=ORIENTED_EDGE('',*,*,#8975,.F.);
#13069=ORIENTED_EDGE('',*,*,#8976,.T.);
#13070=ORIENTED_EDGE('',*,*,#8977,.T.);
#13071=ORIENTED_EDGE('',*,*,#8978,.T.);
#13072=ORIENTED_EDGE('',*,*,#8979,.T.);
#13073=ORIENTED_EDGE('',*,*,#8977,.F.);
#13074=ORIENTED_EDGE('',*,*,#8980,.T.);
#13075=ORIENTED_EDGE('',*,*,#8981,.F.);
#13076=ORIENTED_EDGE('',*,*,#8982,.T.);
#13077=ORIENTED_EDGE('',*,*,#8976,.F.);
#13078=ORIENTED_EDGE('',*,*,#8983,.F.);
#13079=ORIENTED_EDGE('',*,*,#8984,.F.);
#13080=ORIENTED_EDGE('',*,*,#8985,.F.);
#13081=ORIENTED_EDGE('',*,*,#8986,.F.);
#13082=ORIENTED_EDGE('',*,*,#8987,.F.);
#13083=ORIENTED_EDGE('',*,*,#8988,.T.);
#13084=ORIENTED_EDGE('',*,*,#8989,.F.);
#13085=ORIENTED_EDGE('',*,*,#8988,.F.);
#13086=ORIENTED_EDGE('',*,*,#8990,.F.);
#13087=ORIENTED_EDGE('',*,*,#8991,.F.);
#13088=ORIENTED_EDGE('',*,*,#8992,.F.);
#13089=ORIENTED_EDGE('',*,*,#8993,.F.);
#13090=ORIENTED_EDGE('',*,*,#8994,.F.);
#13091=ORIENTED_EDGE('',*,*,#8995,.F.);
#13092=ORIENTED_EDGE('',*,*,#8980,.F.);
#13093=ORIENTED_EDGE('',*,*,#8996,.T.);
#13094=ORIENTED_EDGE('',*,*,#8997,.T.);
#13095=ORIENTED_EDGE('',*,*,#8998,.T.);
#13096=ORIENTED_EDGE('',*,*,#8997,.F.);
#13097=ORIENTED_EDGE('',*,*,#8998,.F.);
#13098=ORIENTED_EDGE('',*,*,#8999,.T.);
#13099=ORIENTED_EDGE('',*,*,#9000,.F.);
#13100=ORIENTED_EDGE('',*,*,#8999,.F.);
#13101=ORIENTED_EDGE('',*,*,#9001,.T.);
#13102=ORIENTED_EDGE('',*,*,#8996,.F.);
#13103=ORIENTED_EDGE('',*,*,#9002,.T.);
#13104=ORIENTED_EDGE('',*,*,#9003,.T.);
#13105=ORIENTED_EDGE('',*,*,#9000,.T.);
#13106=ORIENTED_EDGE('',*,*,#9003,.F.);
#13107=ORIENTED_EDGE('',*,*,#8989,.T.);
#13108=ORIENTED_EDGE('',*,*,#9002,.F.);
#13109=ORIENTED_EDGE('',*,*,#8984,.T.);
#13110=ORIENTED_EDGE('',*,*,#9004,.T.);
#13111=ORIENTED_EDGE('',*,*,#9005,.T.);
#13112=ORIENTED_EDGE('',*,*,#9006,.T.);
#13113=ORIENTED_EDGE('',*,*,#9006,.F.);
#13114=ORIENTED_EDGE('',*,*,#9007,.T.);
#13115=ORIENTED_EDGE('',*,*,#9008,.F.);
#13116=ORIENTED_EDGE('',*,*,#8985,.T.);
#13117=ORIENTED_EDGE('',*,*,#9001,.F.);
#13118=ORIENTED_EDGE('',*,*,#9009,.T.);
#13119=ORIENTED_EDGE('',*,*,#9010,.F.);
#13120=ORIENTED_EDGE('',*,*,#9011,.F.);
#13121=ORIENTED_EDGE('',*,*,#9007,.F.);
#13122=ORIENTED_EDGE('',*,*,#9005,.F.);
#13123=ORIENTED_EDGE('',*,*,#9012,.F.);
#13124=ORIENTED_EDGE('',*,*,#8978,.F.);
#13125=ORIENTED_EDGE('',*,*,#8982,.F.);
#13126=ORIENTED_EDGE('',*,*,#9013,.F.);
#13127=ORIENTED_EDGE('',*,*,#9014,.F.);
#13128=ORIENTED_EDGE('',*,*,#9015,.F.);
#13129=ORIENTED_EDGE('',*,*,#9016,.F.);
#13130=ORIENTED_EDGE('',*,*,#9017,.F.);
#13131=ORIENTED_EDGE('',*,*,#9018,.F.);
#13132=ORIENTED_EDGE('',*,*,#9009,.F.);
#13133=ORIENTED_EDGE('',*,*,#8986,.T.);
#13134=ORIENTED_EDGE('',*,*,#9008,.T.);
#13135=ORIENTED_EDGE('',*,*,#9011,.T.);
#13136=ORIENTED_EDGE('',*,*,#9019,.T.);
#13137=ORIENTED_EDGE('',*,*,#9019,.F.);
#13138=ORIENTED_EDGE('',*,*,#9010,.T.);
#13139=ORIENTED_EDGE('',*,*,#9018,.T.);
#13140=ORIENTED_EDGE('',*,*,#9020,.F.);
#13141=ORIENTED_EDGE('',*,*,#8990,.T.);
#13142=ORIENTED_EDGE('',*,*,#8987,.T.);
#13143=ORIENTED_EDGE('',*,*,#8991,.T.);
#13144=ORIENTED_EDGE('',*,*,#9020,.T.);
#13145=ORIENTED_EDGE('',*,*,#9017,.T.);
#13146=ORIENTED_EDGE('',*,*,#9021,.T.);
#13147=ORIENTED_EDGE('',*,*,#8995,.T.);
#13148=ORIENTED_EDGE('',*,*,#9022,.T.);
#13149=ORIENTED_EDGE('',*,*,#9013,.T.);
#13150=ORIENTED_EDGE('',*,*,#8981,.T.);
#13151=ORIENTED_EDGE('',*,*,#9022,.F.);
#13152=ORIENTED_EDGE('',*,*,#8994,.T.);
#13153=ORIENTED_EDGE('',*,*,#9023,.F.);
#13154=ORIENTED_EDGE('',*,*,#9014,.T.);
#13155=ORIENTED_EDGE('',*,*,#8993,.T.);
#13156=ORIENTED_EDGE('',*,*,#9024,.T.);
#13157=ORIENTED_EDGE('',*,*,#9015,.T.);
#13158=ORIENTED_EDGE('',*,*,#9023,.T.);
#13159=ORIENTED_EDGE('',*,*,#9021,.F.);
#13160=ORIENTED_EDGE('',*,*,#9016,.T.);
#13161=ORIENTED_EDGE('',*,*,#9024,.F.);
#13162=ORIENTED_EDGE('',*,*,#8992,.T.);
#13163=ORIENTED_EDGE('',*,*,#8979,.F.);
#13164=ORIENTED_EDGE('',*,*,#9012,.T.);
#13165=ORIENTED_EDGE('',*,*,#9004,.F.);
#13166=ORIENTED_EDGE('',*,*,#8983,.T.);
#13167=ORIENTED_EDGE('',*,*,#9025,.F.);
#13168=ORIENTED_EDGE('',*,*,#9026,.T.);
#13169=ORIENTED_EDGE('',*,*,#9027,.T.);
#13170=ORIENTED_EDGE('',*,*,#9028,.T.);
#13171=ORIENTED_EDGE('',*,*,#9029,.F.);
#13172=ORIENTED_EDGE('',*,*,#9030,.T.);
#13173=ORIENTED_EDGE('',*,*,#9025,.T.);
#13174=ORIENTED_EDGE('',*,*,#9031,.T.);
#13175=ORIENTED_EDGE('',*,*,#9032,.F.);
#13176=ORIENTED_EDGE('',*,*,#9033,.T.);
#13177=ORIENTED_EDGE('',*,*,#9029,.T.);
#13178=ORIENTED_EDGE('',*,*,#9034,.T.);
#13179=ORIENTED_EDGE('',*,*,#9035,.F.);
#13180=ORIENTED_EDGE('',*,*,#9036,.T.);
#13181=ORIENTED_EDGE('',*,*,#9032,.T.);
#13182=ORIENTED_EDGE('',*,*,#9037,.T.);
#13183=ORIENTED_EDGE('',*,*,#9038,.F.);
#13184=ORIENTED_EDGE('',*,*,#9039,.T.);
#13185=ORIENTED_EDGE('',*,*,#9035,.T.);
#13186=ORIENTED_EDGE('',*,*,#9040,.T.);
#13187=ORIENTED_EDGE('',*,*,#9041,.F.);
#13188=ORIENTED_EDGE('',*,*,#9042,.T.);
#13189=ORIENTED_EDGE('',*,*,#9038,.T.);
#13190=ORIENTED_EDGE('',*,*,#9043,.T.);
#13191=ORIENTED_EDGE('',*,*,#9044,.F.);
#13192=ORIENTED_EDGE('',*,*,#9045,.T.);
#13193=ORIENTED_EDGE('',*,*,#9041,.T.);
#13194=ORIENTED_EDGE('',*,*,#9046,.T.);
#13195=ORIENTED_EDGE('',*,*,#9047,.F.);
#13196=ORIENTED_EDGE('',*,*,#9048,.T.);
#13197=ORIENTED_EDGE('',*,*,#9044,.T.);
#13198=ORIENTED_EDGE('',*,*,#9049,.T.);
#13199=ORIENTED_EDGE('',*,*,#9050,.F.);
#13200=ORIENTED_EDGE('',*,*,#9051,.T.);
#13201=ORIENTED_EDGE('',*,*,#9047,.T.);
#13202=ORIENTED_EDGE('',*,*,#9052,.T.);
#13203=ORIENTED_EDGE('',*,*,#9053,.F.);
#13204=ORIENTED_EDGE('',*,*,#9054,.T.);
#13205=ORIENTED_EDGE('',*,*,#9050,.T.);
#13206=ORIENTED_EDGE('',*,*,#9055,.T.);
#13207=ORIENTED_EDGE('',*,*,#9056,.F.);
#13208=ORIENTED_EDGE('',*,*,#9057,.T.);
#13209=ORIENTED_EDGE('',*,*,#9053,.T.);
#13210=ORIENTED_EDGE('',*,*,#9058,.T.);
#13211=ORIENTED_EDGE('',*,*,#9059,.F.);
#13212=ORIENTED_EDGE('',*,*,#9060,.T.);
#13213=ORIENTED_EDGE('',*,*,#9056,.T.);
#13214=ORIENTED_EDGE('',*,*,#9061,.T.);
#13215=ORIENTED_EDGE('',*,*,#9062,.F.);
#13216=ORIENTED_EDGE('',*,*,#9063,.T.);
#13217=ORIENTED_EDGE('',*,*,#9059,.T.);
#13218=ORIENTED_EDGE('',*,*,#9064,.T.);
#13219=ORIENTED_EDGE('',*,*,#9065,.F.);
#13220=ORIENTED_EDGE('',*,*,#9066,.T.);
#13221=ORIENTED_EDGE('',*,*,#9062,.T.);
#13222=ORIENTED_EDGE('',*,*,#9067,.T.);
#13223=ORIENTED_EDGE('',*,*,#9068,.F.);
#13224=ORIENTED_EDGE('',*,*,#9069,.T.);
#13225=ORIENTED_EDGE('',*,*,#9065,.T.);
#13226=ORIENTED_EDGE('',*,*,#9070,.T.);
#13227=ORIENTED_EDGE('',*,*,#9071,.F.);
#13228=ORIENTED_EDGE('',*,*,#9072,.T.);
#13229=ORIENTED_EDGE('',*,*,#9068,.T.);
#13230=ORIENTED_EDGE('',*,*,#9073,.T.);
#13231=ORIENTED_EDGE('',*,*,#9074,.F.);
#13232=ORIENTED_EDGE('',*,*,#9075,.T.);
#13233=ORIENTED_EDGE('',*,*,#9071,.T.);
#13234=ORIENTED_EDGE('',*,*,#9076,.T.);
#13235=ORIENTED_EDGE('',*,*,#9077,.F.);
#13236=ORIENTED_EDGE('',*,*,#9078,.F.);
#13237=ORIENTED_EDGE('',*,*,#9079,.T.);
#13238=ORIENTED_EDGE('',*,*,#9074,.T.);
#13239=ORIENTED_EDGE('',*,*,#9080,.T.);
#13240=ORIENTED_EDGE('',*,*,#9081,.F.);
#13241=ORIENTED_EDGE('',*,*,#9082,.T.);
#13242=ORIENTED_EDGE('',*,*,#9083,.F.);
#13243=ORIENTED_EDGE('',*,*,#9084,.F.);
#13244=ORIENTED_EDGE('',*,*,#9085,.F.);
#13245=ORIENTED_EDGE('',*,*,#9086,.T.);
#13246=ORIENTED_EDGE('',*,*,#9081,.T.);
#13247=ORIENTED_EDGE('',*,*,#9087,.F.);
#13248=ORIENTED_EDGE('',*,*,#9088,.F.);
#13249=ORIENTED_EDGE('',*,*,#9089,.T.);
#13250=ORIENTED_EDGE('',*,*,#9085,.T.);
#13251=ORIENTED_EDGE('',*,*,#9090,.F.);
#13252=ORIENTED_EDGE('',*,*,#9091,.F.);
#13253=ORIENTED_EDGE('',*,*,#9092,.T.);
#13254=ORIENTED_EDGE('',*,*,#9088,.T.);
#13255=ORIENTED_EDGE('',*,*,#9093,.F.);
#13256=ORIENTED_EDGE('',*,*,#9094,.F.);
#13257=ORIENTED_EDGE('',*,*,#9095,.T.);
#13258=ORIENTED_EDGE('',*,*,#9091,.T.);
#13259=ORIENTED_EDGE('',*,*,#9096,.F.);
#13260=ORIENTED_EDGE('',*,*,#9097,.F.);
#13261=ORIENTED_EDGE('',*,*,#9098,.T.);
#13262=ORIENTED_EDGE('',*,*,#9094,.T.);
#13263=ORIENTED_EDGE('',*,*,#9099,.F.);
#13264=ORIENTED_EDGE('',*,*,#9100,.F.);
#13265=ORIENTED_EDGE('',*,*,#9101,.T.);
#13266=ORIENTED_EDGE('',*,*,#9097,.T.);
#13267=ORIENTED_EDGE('',*,*,#9102,.F.);
#13268=ORIENTED_EDGE('',*,*,#9103,.F.);
#13269=ORIENTED_EDGE('',*,*,#9104,.T.);
#13270=ORIENTED_EDGE('',*,*,#9100,.T.);
#13271=ORIENTED_EDGE('',*,*,#9105,.F.);
#13272=ORIENTED_EDGE('',*,*,#9106,.F.);
#13273=ORIENTED_EDGE('',*,*,#9107,.T.);
#13274=ORIENTED_EDGE('',*,*,#9103,.T.);
#13275=ORIENTED_EDGE('',*,*,#9108,.F.);
#13276=ORIENTED_EDGE('',*,*,#9109,.F.);
#13277=ORIENTED_EDGE('',*,*,#9110,.T.);
#13278=ORIENTED_EDGE('',*,*,#9106,.T.);
#13279=ORIENTED_EDGE('',*,*,#9111,.F.);
#13280=ORIENTED_EDGE('',*,*,#9112,.F.);
#13281=ORIENTED_EDGE('',*,*,#9113,.T.);
#13282=ORIENTED_EDGE('',*,*,#9109,.T.);
#13283=ORIENTED_EDGE('',*,*,#9114,.F.);
#13284=ORIENTED_EDGE('',*,*,#9115,.F.);
#13285=ORIENTED_EDGE('',*,*,#9116,.T.);
#13286=ORIENTED_EDGE('',*,*,#9112,.T.);
#13287=ORIENTED_EDGE('',*,*,#9117,.F.);
#13288=ORIENTED_EDGE('',*,*,#9118,.F.);
#13289=ORIENTED_EDGE('',*,*,#9119,.T.);
#13290=ORIENTED_EDGE('',*,*,#9115,.T.);
#13291=ORIENTED_EDGE('',*,*,#9120,.F.);
#13292=ORIENTED_EDGE('',*,*,#9121,.F.);
#13293=ORIENTED_EDGE('',*,*,#9122,.T.);
#13294=ORIENTED_EDGE('',*,*,#9118,.T.);
#13295=ORIENTED_EDGE('',*,*,#9123,.F.);
#13296=ORIENTED_EDGE('',*,*,#9124,.F.);
#13297=ORIENTED_EDGE('',*,*,#9125,.T.);
#13298=ORIENTED_EDGE('',*,*,#9121,.T.);
#13299=ORIENTED_EDGE('',*,*,#9126,.F.);
#13300=ORIENTED_EDGE('',*,*,#9127,.F.);
#13301=ORIENTED_EDGE('',*,*,#9128,.T.);
#13302=ORIENTED_EDGE('',*,*,#9124,.T.);
#13303=ORIENTED_EDGE('',*,*,#9129,.F.);
#13304=ORIENTED_EDGE('',*,*,#9130,.F.);
#13305=ORIENTED_EDGE('',*,*,#9131,.T.);
#13306=ORIENTED_EDGE('',*,*,#9127,.T.);
#13307=ORIENTED_EDGE('',*,*,#9132,.F.);
#13308=ORIENTED_EDGE('',*,*,#9133,.F.);
#13309=ORIENTED_EDGE('',*,*,#9134,.F.);
#13310=ORIENTED_EDGE('',*,*,#9080,.F.);
#13311=ORIENTED_EDGE('',*,*,#9076,.F.);
#13312=ORIENTED_EDGE('',*,*,#9073,.F.);
#13313=ORIENTED_EDGE('',*,*,#9070,.F.);
#13314=ORIENTED_EDGE('',*,*,#9067,.F.);
#13315=ORIENTED_EDGE('',*,*,#9064,.F.);
#13316=ORIENTED_EDGE('',*,*,#9061,.F.);
#13317=ORIENTED_EDGE('',*,*,#9058,.F.);
#13318=ORIENTED_EDGE('',*,*,#9055,.F.);
#13319=ORIENTED_EDGE('',*,*,#9052,.F.);
#13320=ORIENTED_EDGE('',*,*,#9049,.F.);
#13321=ORIENTED_EDGE('',*,*,#9046,.F.);
#13322=ORIENTED_EDGE('',*,*,#9043,.F.);
#13323=ORIENTED_EDGE('',*,*,#9040,.F.);
#13324=ORIENTED_EDGE('',*,*,#9037,.F.);
#13325=ORIENTED_EDGE('',*,*,#9034,.F.);
#13326=ORIENTED_EDGE('',*,*,#9031,.F.);
#13327=ORIENTED_EDGE('',*,*,#9028,.F.);
#13328=ORIENTED_EDGE('',*,*,#9135,.F.);
#13329=ORIENTED_EDGE('',*,*,#9136,.T.);
#13330=ORIENTED_EDGE('',*,*,#9132,.T.);
#13331=ORIENTED_EDGE('',*,*,#9129,.T.);
#13332=ORIENTED_EDGE('',*,*,#9126,.T.);
#13333=ORIENTED_EDGE('',*,*,#9123,.T.);
#13334=ORIENTED_EDGE('',*,*,#9120,.T.);
#13335=ORIENTED_EDGE('',*,*,#9117,.T.);
#13336=ORIENTED_EDGE('',*,*,#9114,.T.);
#13337=ORIENTED_EDGE('',*,*,#9111,.T.);
#13338=ORIENTED_EDGE('',*,*,#9108,.T.);
#13339=ORIENTED_EDGE('',*,*,#9105,.T.);
#13340=ORIENTED_EDGE('',*,*,#9102,.T.);
#13341=ORIENTED_EDGE('',*,*,#9099,.T.);
#13342=ORIENTED_EDGE('',*,*,#9096,.T.);
#13343=ORIENTED_EDGE('',*,*,#9093,.T.);
#13344=ORIENTED_EDGE('',*,*,#9090,.T.);
#13345=ORIENTED_EDGE('',*,*,#9087,.T.);
#13346=ORIENTED_EDGE('',*,*,#9084,.T.);
#13347=ORIENTED_EDGE('',*,*,#9137,.T.);
#13348=ORIENTED_EDGE('',*,*,#9138,.T.);
#13349=ORIENTED_EDGE('',*,*,#9139,.T.);
#13350=ORIENTED_EDGE('',*,*,#9140,.T.);
#13351=ORIENTED_EDGE('',*,*,#9135,.T.);
#13352=ORIENTED_EDGE('',*,*,#9130,.T.);
#13353=ORIENTED_EDGE('',*,*,#9136,.F.);
#13354=ORIENTED_EDGE('',*,*,#9140,.F.);
#13355=ORIENTED_EDGE('',*,*,#9141,.T.);
#13356=ORIENTED_EDGE('',*,*,#9142,.F.);
#13357=ORIENTED_EDGE('',*,*,#9082,.F.);
#13358=ORIENTED_EDGE('',*,*,#9086,.F.);
#13359=ORIENTED_EDGE('',*,*,#9089,.F.);
#13360=ORIENTED_EDGE('',*,*,#9092,.F.);
#13361=ORIENTED_EDGE('',*,*,#9095,.F.);
#13362=ORIENTED_EDGE('',*,*,#9098,.F.);
#13363=ORIENTED_EDGE('',*,*,#9101,.F.);
#13364=ORIENTED_EDGE('',*,*,#9104,.F.);
#13365=ORIENTED_EDGE('',*,*,#9107,.F.);
#13366=ORIENTED_EDGE('',*,*,#9110,.F.);
#13367=ORIENTED_EDGE('',*,*,#9113,.F.);
#13368=ORIENTED_EDGE('',*,*,#9116,.F.);
#13369=ORIENTED_EDGE('',*,*,#9119,.F.);
#13370=ORIENTED_EDGE('',*,*,#9122,.F.);
#13371=ORIENTED_EDGE('',*,*,#9125,.F.);
#13372=ORIENTED_EDGE('',*,*,#9128,.F.);
#13373=ORIENTED_EDGE('',*,*,#9131,.F.);
#13374=ORIENTED_EDGE('',*,*,#9141,.F.);
#13375=ORIENTED_EDGE('',*,*,#9139,.F.);
#13376=ORIENTED_EDGE('',*,*,#9026,.F.);
#13377=ORIENTED_EDGE('',*,*,#9030,.F.);
#13378=ORIENTED_EDGE('',*,*,#9033,.F.);
#13379=ORIENTED_EDGE('',*,*,#9036,.F.);
#13380=ORIENTED_EDGE('',*,*,#9039,.F.);
#13381=ORIENTED_EDGE('',*,*,#9042,.F.);
#13382=ORIENTED_EDGE('',*,*,#9045,.F.);
#13383=ORIENTED_EDGE('',*,*,#9048,.F.);
#13384=ORIENTED_EDGE('',*,*,#9051,.F.);
#13385=ORIENTED_EDGE('',*,*,#9054,.F.);
#13386=ORIENTED_EDGE('',*,*,#9057,.F.);
#13387=ORIENTED_EDGE('',*,*,#9060,.F.);
#13388=ORIENTED_EDGE('',*,*,#9063,.F.);
#13389=ORIENTED_EDGE('',*,*,#9066,.F.);
#13390=ORIENTED_EDGE('',*,*,#9069,.F.);
#13391=ORIENTED_EDGE('',*,*,#9072,.F.);
#13392=ORIENTED_EDGE('',*,*,#9075,.F.);
#13393=ORIENTED_EDGE('',*,*,#9079,.F.);
#13394=ORIENTED_EDGE('',*,*,#9143,.T.);
#13395=ORIENTED_EDGE('',*,*,#9144,.F.);
#13396=ORIENTED_EDGE('',*,*,#9143,.F.);
#13397=ORIENTED_EDGE('',*,*,#9145,.F.);
#13398=ORIENTED_EDGE('',*,*,#9146,.T.);
#13399=ORIENTED_EDGE('',*,*,#9147,.T.);
#13400=ORIENTED_EDGE('',*,*,#9148,.F.);
#13401=ORIENTED_EDGE('',*,*,#9149,.F.);
#13402=ORIENTED_EDGE('',*,*,#9148,.T.);
#13403=ORIENTED_EDGE('',*,*,#9150,.T.);
#13404=ORIENTED_EDGE('',*,*,#9151,.F.);
#13405=ORIENTED_EDGE('',*,*,#9152,.F.);
#13406=ORIENTED_EDGE('',*,*,#9151,.T.);
#13407=ORIENTED_EDGE('',*,*,#9153,.T.);
#13408=ORIENTED_EDGE('',*,*,#9154,.F.);
#13409=ORIENTED_EDGE('',*,*,#9155,.F.);
#13410=ORIENTED_EDGE('',*,*,#9154,.T.);
#13411=ORIENTED_EDGE('',*,*,#9156,.T.);
#13412=ORIENTED_EDGE('',*,*,#9157,.F.);
#13413=ORIENTED_EDGE('',*,*,#9158,.F.);
#13414=ORIENTED_EDGE('',*,*,#9159,.T.);
#13415=ORIENTED_EDGE('',*,*,#9160,.T.);
#13416=ORIENTED_EDGE('',*,*,#9146,.F.);
#13417=ORIENTED_EDGE('',*,*,#9161,.F.);
#13418=ORIENTED_EDGE('',*,*,#9157,.T.);
#13419=ORIENTED_EDGE('',*,*,#9162,.T.);
#13420=ORIENTED_EDGE('',*,*,#9159,.F.);
#13421=ORIENTED_EDGE('',*,*,#9162,.F.);
#13422=ORIENTED_EDGE('',*,*,#9156,.F.);
#13423=ORIENTED_EDGE('',*,*,#9153,.F.);
#13424=ORIENTED_EDGE('',*,*,#9150,.F.);
#13425=ORIENTED_EDGE('',*,*,#9147,.F.);
#13426=ORIENTED_EDGE('',*,*,#9160,.F.);
#13427=ORIENTED_EDGE('',*,*,#9144,.T.);
#13428=ORIENTED_EDGE('',*,*,#9163,.F.);
#13429=ORIENTED_EDGE('',*,*,#9137,.F.);
#13430=ORIENTED_EDGE('',*,*,#9027,.F.);
#13431=ORIENTED_EDGE('',*,*,#9138,.F.);
#13432=ORIENTED_EDGE('',*,*,#9164,.T.);
#13433=ORIENTED_EDGE('',*,*,#9163,.T.);
#13434=ORIENTED_EDGE('',*,*,#9164,.F.);
#13435=ORIENTED_EDGE('',*,*,#9077,.T.);
#13436=ORIENTED_EDGE('',*,*,#9134,.T.);
#13437=ORIENTED_EDGE('',*,*,#9165,.F.);
#13438=ORIENTED_EDGE('',*,*,#9166,.F.);
#13439=ORIENTED_EDGE('',*,*,#9078,.T.);
#13440=ORIENTED_EDGE('',*,*,#9165,.T.);
#13441=ORIENTED_EDGE('',*,*,#9133,.T.);
#13442=ORIENTED_EDGE('',*,*,#9083,.T.);
#13443=ORIENTED_EDGE('',*,*,#9142,.T.);
#13444=ORIENTED_EDGE('',*,*,#9167,.F.);
#13445=ORIENTED_EDGE('',*,*,#9168,.T.);
#13446=ORIENTED_EDGE('',*,*,#9166,.T.);
#13447=ORIENTED_EDGE('',*,*,#9168,.F.);
#13448=ORIENTED_EDGE('',*,*,#9169,.F.);
#13449=ORIENTED_EDGE('',*,*,#9155,.T.);
#13450=ORIENTED_EDGE('',*,*,#9161,.T.);
#13451=ORIENTED_EDGE('',*,*,#9158,.T.);
#13452=ORIENTED_EDGE('',*,*,#9145,.T.);
#13453=ORIENTED_EDGE('',*,*,#9149,.T.);
#13454=ORIENTED_EDGE('',*,*,#9152,.T.);
#13455=ORIENTED_EDGE('',*,*,#9170,.T.);
#13456=ORIENTED_EDGE('',*,*,#9169,.T.);
#13457=ORIENTED_EDGE('',*,*,#9167,.T.);
#13458=ORIENTED_EDGE('',*,*,#9170,.F.);
#13459=PLANE('',#14935);
#13460=PLANE('',#14936);
#13461=PLANE('',#14942);
#13462=PLANE('',#14943);
#13463=PLANE('',#14944);
#13464=PLANE('',#14948);
#13465=PLANE('',#14949);
#13466=PLANE('',#14950);
#13467=PLANE('',#14951);
#13468=PLANE('',#14955);
#13469=PLANE('',#14956);
#13470=PLANE('',#14960);
#13471=PLANE('',#14962);
#13472=PLANE('',#14964);
#13473=PLANE('',#14965);
#13474=PLANE('',#14966);
#13475=PLANE('',#14967);
#13476=PLANE('',#14968);
#13477=PLANE('',#14969);
#13478=PLANE('',#14972);
#13479=PLANE('',#14973);
#13480=PLANE('',#14974);
#13481=PLANE('',#14978);
#13482=PLANE('',#14980);
#13483=PLANE('',#14992);
#13484=PLANE('',#14994);
#13485=PLANE('',#14995);
#13486=PLANE('',#14996);
#13487=PLANE('',#14998);
#13488=PLANE('',#15002);
#13489=PLANE('',#15006);
#13490=PLANE('',#15007);
#13491=PLANE('',#15008);
#13492=PLANE('',#15010);
#13493=PLANE('',#15011);
#13494=PLANE('',#15012);
#13495=PLANE('',#15013);
#13496=PLANE('',#15017);
#13497=PLANE('',#15021);
#13498=PLANE('',#15025);
#13499=PLANE('',#15029);
#13500=PLANE('',#15030);
#13501=PLANE('',#15035);
#13502=PLANE('',#15037);
#13503=PLANE('',#15041);
#13504=PLANE('',#15042);
#13505=PLANE('',#15043);
#13506=PLANE('',#15044);
#13507=PLANE('',#15045);
#13508=PLANE('',#15046);
#13509=PLANE('',#15049);
#13510=PLANE('',#15050);
#13511=PLANE('',#15053);
#13512=PLANE('',#15054);
#13513=PLANE('',#15055);
#13514=PLANE('',#15056);
#13515=PLANE('',#15058);
#13516=PLANE('',#15060);
#13517=PLANE('',#15061);
#13518=PLANE('',#15065);
#13519=PLANE('',#15069);
#13520=PLANE('',#15070);
#13521=PLANE('',#15072);
#13522=PLANE('',#15074);
#13523=PLANE('',#15075);
#13524=PLANE('',#15079);
#13525=PLANE('',#15083);
#13526=PLANE('',#15084);
#13527=PLANE('',#15086);
#13528=PLANE('',#15087);
#13529=PLANE('',#15088);
#13530=PLANE('',#15091);
#13531=PLANE('',#15097);
#13532=PLANE('',#15098);
#13533=PLANE('',#15099);
#13534=PLANE('',#15104);
#13535=PLANE('',#15106);
#13536=PLANE('',#15107);
#13537=PLANE('',#15108);
#13538=PLANE('',#15114);
#13539=PLANE('',#15115);
#13540=PLANE('',#15120);
#13541=PLANE('',#15123);
#13542=PLANE('',#15124);
#13543=PLANE('',#15134);
#13544=PLANE('',#15135);
#13545=PLANE('',#15136);
#13546=PLANE('',#15138);
#13547=PLANE('',#15142);
#13548=PLANE('',#15143);
#13549=PLANE('',#15146);
#13550=PLANE('',#15147);
#13551=PLANE('',#15150);
#13552=PLANE('',#15151);
#13553=PLANE('',#15152);
#13554=PLANE('',#15156);
#13555=PLANE('',#15157);
#13556=PLANE('',#15160);
#13557=PLANE('',#15161);
#13558=PLANE('',#15162);
#13559=PLANE('',#15163);
#13560=PLANE('',#15164);
#13561=PLANE('',#15165);
#13562=PLANE('',#15166);
#13563=PLANE('',#15167);
#13564=PLANE('',#15173);
#13565=PLANE('',#15179);
#13566=PLANE('',#15182);
#13567=PLANE('',#15183);
#13568=PLANE('',#15184);
#13569=PLANE('',#15185);
#13570=PLANE('',#15186);
#13571=PLANE('',#15187);
#13572=PLANE('',#15188);
#13573=PLANE('',#15189);
#13574=PLANE('',#15190);
#13575=PLANE('',#15191);
#13576=PLANE('',#15194);
#13577=PLANE('',#15195);
#13578=PLANE('',#15198);
#13579=PLANE('',#15199);
#13580=PLANE('',#15200);
#13581=PLANE('',#15201);
#13582=PLANE('',#15202);
#13583=PLANE('',#15203);
#13584=PLANE('',#15204);
#13585=PLANE('',#15205);
#13586=PLANE('',#15206);
#13587=PLANE('',#15207);
#13588=PLANE('',#15208);
#13589=PLANE('',#15209);
#13590=PLANE('',#15210);
#13591=PLANE('',#15211);
#13592=PLANE('',#15212);
#13593=PLANE('',#15213);
#13594=PLANE('',#15214);
#13595=PLANE('',#15215);
#13596=PLANE('',#15216);
#13597=PLANE('',#15217);
#13598=PLANE('',#15218);
#13599=PLANE('',#15219);
#13600=PLANE('',#15220);
#13601=PLANE('',#15221);
#13602=PLANE('',#15222);
#13603=PLANE('',#15223);
#13604=PLANE('',#15224);
#13605=PLANE('',#15225);
#13606=PLANE('',#15226);
#13607=PLANE('',#15227);
#13608=PLANE('',#15228);
#13609=PLANE('',#15229);
#13610=PLANE('',#15230);
#13611=PLANE('',#15231);
#13612=PLANE('',#15232);
#13613=PLANE('',#15233);
#13614=PLANE('',#15234);
#13615=PLANE('',#15235);
#13616=PLANE('',#15236);
#13617=PLANE('',#15237);
#13618=PLANE('',#15238);
#13619=PLANE('',#15241);
#13620=PLANE('',#15245);
#13621=PLANE('',#15249);
#13622=PLANE('',#15253);
#13623=PLANE('',#15259);
#13624=PLANE('',#15263);
#13625=PLANE('',#15264);
#13626=PLANE('',#15265);
#13627=PLANE('',#15266);
#13628=PLANE('',#15267);
#13629=PLANE('',#15271);
#13630=PLANE('',#15275);
#13631=PLANE('',#15278);
#13632=PLANE('',#15281);
#13633=PLANE('',#15282);
#13634=PLANE('',#15283);
#13635=PLANE('',#15284);
#13636=PLANE('',#15285);
#13637=PLANE('',#15286);
#13638=PLANE('',#15287);
#13639=PLANE('',#15289);
#13640=PLANE('',#15291);
#13641=PLANE('',#15292);
#13642=PLANE('',#15293);
#13643=PLANE('',#15294);
#13644=PLANE('',#15295);
#13645=PLANE('',#15311);
#13646=PLANE('',#15312);
#13647=PLANE('',#15313);
#13648=PLANE('',#15314);
#13649=PLANE('',#15315);
#13650=PLANE('',#15316);
#13651=PLANE('',#15317);
#13652=PLANE('',#15318);
#13653=PLANE('',#15319);
#13654=PLANE('',#15320);
#13655=PLANE('',#15321);
#13656=PLANE('',#15322);
#13657=PLANE('',#15329);
#13658=PLANE('',#15338);
#13659=PLANE('',#15345);
#13660=PLANE('',#15348);
#13661=PLANE('',#15351);
#13662=PLANE('',#15354);
#13663=PLANE('',#15359);
#13664=PLANE('',#15362);
#13665=PLANE('',#15363);
#13666=PLANE('',#15366);
#13667=PLANE('',#15369);
#13668=PLANE('',#15373);
#13669=PLANE('',#15379);
#13670=PLANE('',#15382);
#13671=PLANE('',#15383);
#13672=PLANE('',#15384);
#13673=PLANE('',#15386);
#13674=PLANE('',#15388);
#13675=PLANE('',#15391);
#13676=PLANE('',#15395);
#13677=PLANE('',#15397);
#13678=PLANE('',#15402);
#13679=PLANE('',#15404);
#13680=PLANE('',#15405);
#13681=PLANE('',#15406);
#13682=PLANE('',#15407);
#13683=PLANE('',#15408);
#13684=PLANE('',#15409);
#13685=PLANE('',#15410);
#13686=PLANE('',#15411);
#13687=PLANE('',#15412);
#13688=PLANE('',#15413);
#13689=PLANE('',#15414);
#13690=PLANE('',#15415);
#13691=PLANE('',#15416);
#13692=PLANE('',#15417);
#13693=PLANE('',#15418);
#13694=PLANE('',#15419);
#13695=PLANE('',#15420);
#13696=PLANE('',#15421);
#13697=PLANE('',#15422);
#13698=PLANE('',#15423);
#13699=PLANE('',#15424);
#13700=PLANE('',#15426);
#13701=PLANE('',#15427);
#13702=PLANE('',#15428);
#13703=PLANE('',#15429);
#13704=PLANE('',#15430);
#13705=PLANE('',#15431);
#13706=PLANE('',#15432);
#13707=PLANE('',#15433);
#13708=PLANE('',#15434);
#13709=PLANE('',#15435);
#13710=PLANE('',#15436);
#13711=PLANE('',#15437);
#13712=PLANE('',#15438);
#13713=PLANE('',#15439);
#13714=PLANE('',#15440);
#13715=PLANE('',#15441);
#13716=PLANE('',#15442);
#13717=PLANE('',#15443);
#13718=PLANE('',#15444);
#13719=PLANE('',#15445);
#13720=PLANE('',#15446);
#13721=PLANE('',#15447);
#13722=PLANE('',#15448);
#13723=PLANE('',#15450);
#13724=PLANE('',#15451);
#13725=PLANE('',#15453);
#13726=PLANE('',#15591);
#13727=PLANE('',#15593);
#13728=PLANE('',#15598);
#13729=PLANE('',#15599);
#13730=PLANE('',#15600);
#13731=PLANE('',#15601);
#13732=PLANE('',#15602);
#13733=PLANE('',#15603);
#13734=PLANE('',#15604);
#13735=PLANE('',#15605);
#13736=PLANE('',#15606);
#13737=PLANE('',#15607);
#13738=PLANE('',#15608);
#13739=PLANE('',#15609);
#13740=PLANE('',#15610);
#13741=PLANE('',#15611);
#13742=PLANE('',#15612);
#13743=PLANE('',#15613);
#13744=PLANE('',#15614);
#13745=PLANE('',#15615);
#13746=PLANE('',#15616);
#13747=PLANE('',#15617);
#13748=PLANE('',#15618);
#13749=PLANE('',#15619);
#13750=PLANE('',#15620);
#13751=PLANE('',#15621);
#13752=PLANE('',#15622);
#13753=PLANE('',#15623);
#13754=PLANE('',#15624);
#13755=PLANE('',#15625);
#13756=PLANE('',#15626);
#13757=PLANE('',#15627);
#13758=PLANE('',#15628);
#13759=PLANE('',#15629);
#13760=PLANE('',#15630);
#13761=PLANE('',#15631);
#13762=PLANE('',#15632);
#13763=PLANE('',#15633);
#13764=PLANE('',#15634);
#13765=PLANE('',#15635);
#13766=PLANE('',#15636);
#13767=PLANE('',#15637);
#13768=PLANE('',#15638);
#13769=PLANE('',#15639);
#13770=PLANE('',#15640);
#13771=PLANE('',#15641);
#13772=PLANE('',#15642);
#13773=PLANE('',#15643);
#13774=PLANE('',#15644);
#13775=PLANE('',#15645);
#13776=PLANE('',#15646);
#13777=PLANE('',#15647);
#13778=PLANE('',#15648);
#13779=PLANE('',#15649);
#13780=PLANE('',#15650);
#13781=PLANE('',#15651);
#13782=PLANE('',#15652);
#13783=PLANE('',#15653);
#13784=PLANE('',#15654);
#13785=PLANE('',#15655);
#13786=PLANE('',#15656);
#13787=PLANE('',#15657);
#13788=PLANE('',#15658);
#13789=PLANE('',#15659);
#13790=PLANE('',#15660);
#13791=PLANE('',#15661);
#13792=PLANE('',#15662);
#13793=PLANE('',#15663);
#13794=PLANE('',#15664);
#13795=PLANE('',#15665);
#13796=PLANE('',#15666);
#13797=PLANE('',#15667);
#13798=PLANE('',#15668);
#13799=PLANE('',#15669);
#13800=PLANE('',#15670);
#13801=PLANE('',#15671);
#13802=PLANE('',#15672);
#13803=PLANE('',#15673);
#13804=PLANE('',#15674);
#13805=PLANE('',#15675);
#13806=PLANE('',#15676);
#13807=PLANE('',#15677);
#13808=PLANE('',#15678);
#13809=PLANE('',#15679);
#13810=PLANE('',#15680);
#13811=PLANE('',#15681);
#13812=PLANE('',#15682);
#13813=PLANE('',#15683);
#13814=PLANE('',#15684);
#13815=PLANE('',#15685);
#13816=PLANE('',#15686);
#13817=PLANE('',#15687);
#13818=PLANE('',#15688);
#13819=PLANE('',#15689);
#13820=PLANE('',#15690);
#13821=PLANE('',#15691);
#13822=PLANE('',#15692);
#13823=PLANE('',#15693);
#13824=PLANE('',#15694);
#13825=PLANE('',#15700);
#13826=PLANE('',#15704);
#13827=PLANE('',#15712);
#13828=PLANE('',#15714);
#13829=PLANE('',#15751);
#13830=PLANE('',#15752);
#13831=PLANE('',#15753);
#13832=PLANE('',#15754);
#13833=PLANE('',#15755);
#13834=PLANE('',#15756);
#13835=PLANE('',#15757);
#13836=PLANE('',#15758);
#13837=PLANE('',#15759);
#13838=PLANE('',#15760);
#13839=PLANE('',#15761);
#13840=PLANE('',#15762);
#13841=PLANE('',#15763);
#13842=PLANE('',#15764);
#13843=PLANE('',#15765);
#13844=PLANE('',#15766);
#13845=PLANE('',#15767);
#13846=PLANE('',#15768);
#13847=PLANE('',#15769);
#13848=PLANE('',#15770);
#13849=PLANE('',#15771);
#13850=PLANE('',#15772);
#13851=PLANE('',#15773);
#13852=PLANE('',#15774);
#13853=PLANE('',#15775);
#13854=PLANE('',#15776);
#13855=PLANE('',#15777);
#13856=PLANE('',#15778);
#13857=PLANE('',#15779);
#13858=PLANE('',#15780);
#13859=PLANE('',#15781);
#13860=PLANE('',#15786);
#13861=PLANE('',#15787);
#13862=PLANE('',#15788);
#13863=PLANE('',#15789);
#13864=PLANE('',#15790);
#13865=PLANE('',#15791);
#13866=PLANE('',#15792);
#13867=PLANE('',#15793);
#13868=PLANE('',#15794);
#13869=PLANE('',#15795);
#13870=PLANE('',#15796);
#13871=PLANE('',#15798);
#13872=PLANE('',#15799);
#13873=PLANE('',#15800);
#13874=PLANE('',#15801);
#13875=PLANE('',#15804);
#13876=PLANE('',#15805);
#13877=PLANE('',#15810);
#13878=PLANE('',#15811);
#13879=PLANE('',#15816);
#13880=PLANE('',#15817);
#13881=PLANE('',#15822);
#13882=PLANE('',#15823);
#13883=PLANE('',#15828);
#13884=PLANE('',#15829);
#13885=PLANE('',#15834);
#13886=PLANE('',#15835);
#13887=PLANE('',#15840);
#13888=PLANE('',#15841);
#13889=PLANE('',#15846);
#13890=PLANE('',#15896);
#13891=PLANE('',#15903);
#13892=PLANE('',#15908);
#13893=PLANE('',#15909);
#13894=PLANE('',#15910);
#13895=PLANE('',#15911);
#13896=PLANE('',#15912);
#13897=PLANE('',#15913);
#13898=PLANE('',#15914);
#13899=PLANE('',#15915);
#13900=PLANE('',#15975);
#13901=PLANE('',#15982);
#13902=PLANE('',#15983);
#13903=PLANE('',#15984);
#13904=PLANE('',#15985);
#13905=PLANE('',#15986);
#13906=PLANE('',#15987);
#13907=PLANE('',#15988);
#13908=PLANE('',#15989);
#13909=PLANE('',#15994);
#13910=PLANE('',#16006);
#13911=PLANE('',#16010);
#13912=PLANE('',#16014);
#13913=PLANE('',#16015);
#13914=PLANE('',#16023);
#13915=PLANE('',#16027);
#13916=PLANE('',#16028);
#13917=PLANE('',#16029);
#13918=PLANE('',#16031);
#13919=PLANE('',#16032);
#13920=PLANE('',#16033);
#13921=PLANE('',#16034);
#13922=PLANE('',#16035);
#13923=PLANE('',#16036);
#13924=PLANE('',#16037);
#13925=PLANE('',#16038);
#13926=PLANE('',#16078);
#13927=PLANE('',#16085);
#13928=PLANE('',#16086);
#13929=PLANE('',#16087);
#13930=PLANE('',#16088);
#13931=PLANE('',#16089);
#13932=PLANE('',#16090);
#13933=PLANE('',#16091);
#13934=PLANE('',#16092);
#13935=PLANE('',#16097);
#13936=ADVANCED_FACE('',(#1368),#13459,.T.);
#13937=ADVANCED_FACE('',(#1369),#13460,.T.);
#13938=ADVANCED_FACE('',(#1370),#1283,.F.);
#13939=ADVANCED_FACE('',(#1371),#690,.F.);
#13940=ADVANCED_FACE('',(#1372),#13461,.T.);
#13941=ADVANCED_FACE('',(#1373),#13462,.T.);
#13942=ADVANCED_FACE('',(#1374),#13463,.T.);
#13943=ADVANCED_FACE('',(#1375),#1284,.T.);
#13944=ADVANCED_FACE('',(#1376),#13464,.T.);
#13945=ADVANCED_FACE('',(#1377),#13465,.T.);
#13946=ADVANCED_FACE('',(#1378),#13466,.T.);
#13947=ADVANCED_FACE('',(#1379),#13467,.T.);
#13948=ADVANCED_FACE('',(#1380),#1285,.T.);
#13949=ADVANCED_FACE('',(#1381),#13468,.T.);
#13950=ADVANCED_FACE('',(#1382),#13469,.F.);
#13951=ADVANCED_FACE('',(#1383),#13470,.T.);
#13952=ADVANCED_FACE('',(#1384),#691,.T.);
#13953=ADVANCED_FACE('',(#1385,#640),#13471,.T.);
#13954=ADVANCED_FACE('',(#1386),#13472,.T.);
#13955=ADVANCED_FACE('',(#1387),#13473,.T.);
#13956=ADVANCED_FACE('',(#1388),#13474,.T.);
#13957=ADVANCED_FACE('',(#1389),#13475,.T.);
#13958=ADVANCED_FACE('',(#1390),#13476,.T.);
#13959=ADVANCED_FACE('',(#1391),#13477,.T.);
#13960=ADVANCED_FACE('',(#1392),#1286,.T.);
#13961=ADVANCED_FACE('',(#1393),#13478,.T.);
#13962=ADVANCED_FACE('',(#1394),#13479,.T.);
#13963=ADVANCED_FACE('',(#1395),#13480,.T.);
#13964=ADVANCED_FACE('',(#1396),#1287,.T.);
#13965=ADVANCED_FACE('',(#1397),#13481,.T.);
#13966=ADVANCED_FACE('',(#1398),#1288,.F.);
#13967=ADVANCED_FACE('',(#1399,#641),#13482,.T.);
#13968=ADVANCED_FACE('',(#1400),#1289,.T.);
#13969=ADVANCED_FACE('',(#1401),#1290,.T.);
#13970=ADVANCED_FACE('',(#1402),#692,.T.);
#13971=ADVANCED_FACE('',(#1403),#693,.F.);
#13972=ADVANCED_FACE('',(#1404),#694,.F.);
#13973=ADVANCED_FACE('',(#1405),#13483,.T.);
#13974=ADVANCED_FACE('',(#1406),#695,.T.);
#13975=ADVANCED_FACE('',(#1407,#642),#13484,.T.);
#13976=ADVANCED_FACE('',(#1408),#13485,.T.);
#13977=ADVANCED_FACE('',(#1409,#643),#13486,.T.);
#13978=ADVANCED_FACE('',(#1410),#13487,.T.);
#13979=ADVANCED_FACE('',(#1411),#1291,.T.);
#13980=ADVANCED_FACE('',(#1412),#13488,.T.);
#13981=ADVANCED_FACE('',(#1413),#1292,.T.);
#13982=ADVANCED_FACE('',(#1414),#13489,.T.);
#13983=ADVANCED_FACE('',(#1415),#13490,.T.);
#13984=ADVANCED_FACE('',(#1416,#644),#13491,.T.);
#13985=ADVANCED_FACE('',(#1417),#13492,.T.);
#13986=ADVANCED_FACE('',(#1418),#13493,.T.);
#13987=ADVANCED_FACE('',(#1419),#13494,.T.);
#13988=ADVANCED_FACE('',(#1420),#13495,.T.);
#13989=ADVANCED_FACE('',(#1421),#1293,.T.);
#13990=ADVANCED_FACE('',(#1422),#13496,.T.);
#13991=ADVANCED_FACE('',(#1423),#1294,.T.);
#13992=ADVANCED_FACE('',(#1424),#13497,.T.);
#13993=ADVANCED_FACE('',(#1425),#1295,.T.);
#13994=ADVANCED_FACE('',(#1426),#13498,.T.);
#13995=ADVANCED_FACE('',(#1427),#1296,.T.);
#13996=ADVANCED_FACE('',(#1428),#13499,.T.);
#13997=ADVANCED_FACE('',(#1429),#13500,.F.);
#13998=ADVANCED_FACE('',(#1430),#696,.T.);
#13999=ADVANCED_FACE('',(#1431),#13501,.T.);
#14000=ADVANCED_FACE('',(#1432),#697,.T.);
#14001=ADVANCED_FACE('',(#1433),#13502,.T.);
#14002=ADVANCED_FACE('',(#1434),#13503,.T.);
#14003=ADVANCED_FACE('',(#1435),#13504,.T.);
#14004=ADVANCED_FACE('',(#1436),#13505,.T.);
#14005=ADVANCED_FACE('',(#1437),#13506,.T.);
#14006=ADVANCED_FACE('',(#1438),#13507,.T.);
#14007=ADVANCED_FACE('',(#1439),#13508,.T.);
#14008=ADVANCED_FACE('',(#1440),#1297,.T.);
#14009=ADVANCED_FACE('',(#1441),#13509,.T.);
#14010=ADVANCED_FACE('',(#1442),#13510,.T.);
#14011=ADVANCED_FACE('',(#1443),#698,.T.);
#14012=ADVANCED_FACE('',(#1444),#13511,.T.);
#14013=ADVANCED_FACE('',(#1445),#13512,.T.);
#14014=ADVANCED_FACE('',(#1446),#13513,.T.);
#14015=ADVANCED_FACE('',(#1447,#645),#13514,.T.);
#14016=ADVANCED_FACE('',(#1448),#13515,.T.);
#14017=ADVANCED_FACE('',(#1449),#1298,.T.);
#14018=ADVANCED_FACE('',(#1450),#13516,.T.);
#14019=ADVANCED_FACE('',(#1451),#13517,.T.);
#14020=ADVANCED_FACE('',(#1452),#1299,.T.);
#14021=ADVANCED_FACE('',(#1453),#13518,.T.);
#14022=ADVANCED_FACE('',(#1454),#1300,.T.);
#14023=ADVANCED_FACE('',(#1455),#13519,.T.);
#14024=ADVANCED_FACE('',(#1456,#646),#13520,.T.);
#14025=ADVANCED_FACE('',(#1457,#647),#13521,.T.);
#14026=ADVANCED_FACE('',(#1458),#13522,.T.);
#14027=ADVANCED_FACE('',(#1459),#13523,.T.);
#14028=ADVANCED_FACE('',(#1460),#1301,.T.);
#14029=ADVANCED_FACE('',(#1461),#13524,.T.);
#14030=ADVANCED_FACE('',(#1462),#1302,.T.);
#14031=ADVANCED_FACE('',(#1463),#13525,.T.);
#14032=ADVANCED_FACE('',(#1464,#648),#13526,.T.);
#14033=ADVANCED_FACE('',(#1465),#13527,.T.);
#14034=ADVANCED_FACE('',(#1466),#13528,.T.);
#14035=ADVANCED_FACE('',(#1467),#13529,.T.);
#14036=ADVANCED_FACE('',(#1468),#1303,.F.);
#14037=ADVANCED_FACE('',(#1469),#13530,.T.);
#14038=ADVANCED_FACE('',(#1470),#1304,.F.);
#14039=ADVANCED_FACE('',(#1471,#649),#699,.F.);
#14040=ADVANCED_FACE('',(#1472),#13531,.T.);
#14041=ADVANCED_FACE('',(#1473),#13532,.T.);
#14042=ADVANCED_FACE('',(#1474),#13533,.T.);
#14043=ADVANCED_FACE('',(#1475),#1305,.F.);
#14044=ADVANCED_FACE('',(#1476),#1306,.F.);
#14045=ADVANCED_FACE('',(#1477),#13534,.T.);
#14046=ADVANCED_FACE('',(#1478),#13535,.F.);
#14047=ADVANCED_FACE('',(#1479),#13536,.T.);
#14048=ADVANCED_FACE('',(#1480),#13537,.T.);
#14049=ADVANCED_FACE('',(#1481),#1307,.T.);
#14050=ADVANCED_FACE('',(#1482),#1308,.T.);
#14051=ADVANCED_FACE('',(#1483),#13538,.F.);
#14052=ADVANCED_FACE('',(#1484),#13539,.F.);
#14053=ADVANCED_FACE('',(#1485,#650),#700,.T.);
#14054=ADVANCED_FACE('',(#1486),#1309,.T.);
#14055=ADVANCED_FACE('',(#1487,#651),#13540,.T.);
#14056=ADVANCED_FACE('',(#1488),#1310,.T.);
#14057=ADVANCED_FACE('',(#1489),#13541,.F.);
#14058=ADVANCED_FACE('',(#1490),#13542,.F.);
#14059=ADVANCED_FACE('',(#1491),#701,.F.);
#14060=ADVANCED_FACE('',(#1492),#702,.F.);
#14061=ADVANCED_FACE('',(#1493),#703,.F.);
#14062=ADVANCED_FACE('',(#1494),#704,.F.);
#14063=ADVANCED_FACE('',(#1495),#705,.T.);
#14064=ADVANCED_FACE('',(#1496),#706,.T.);
#14065=ADVANCED_FACE('',(#1497),#707,.T.);
#14066=ADVANCED_FACE('',(#1498,#652),#13543,.T.);
#14067=ADVANCED_FACE('',(#1499),#13544,.T.);
#14068=ADVANCED_FACE('',(#1500,#653),#13545,.T.);
#14069=ADVANCED_FACE('',(#1501),#13546,.T.);
#14070=ADVANCED_FACE('',(#1502),#1311,.T.);
#14071=ADVANCED_FACE('',(#1503),#13547,.T.);
#14072=ADVANCED_FACE('',(#1504),#13548,.T.);
#14073=ADVANCED_FACE('',(#1505),#708,.T.);
#14074=ADVANCED_FACE('',(#1506),#13549,.T.);
#14075=ADVANCED_FACE('',(#1507),#13550,.T.);
#14076=ADVANCED_FACE('',(#1508),#1312,.T.);
#14077=ADVANCED_FACE('',(#1509),#13551,.T.);
#14078=ADVANCED_FACE('',(#1510,#654),#13552,.F.);
#14079=ADVANCED_FACE('',(#1511),#13553,.T.);
#14080=ADVANCED_FACE('',(#1512),#1313,.T.);
#14081=ADVANCED_FACE('',(#1513),#13554,.T.);
#14082=ADVANCED_FACE('',(#1514),#13555,.T.);
#14083=ADVANCED_FACE('',(#1515),#709,.T.);
#14084=ADVANCED_FACE('',(#1516),#13556,.T.);
#14085=ADVANCED_FACE('',(#1517),#13557,.T.);
#14086=ADVANCED_FACE('',(#1518),#13558,.T.);
#14087=ADVANCED_FACE('',(#1519),#13559,.T.);
#14088=ADVANCED_FACE('',(#1520),#13560,.T.);
#14089=ADVANCED_FACE('',(#1521),#13561,.T.);
#14090=ADVANCED_FACE('',(#1522),#13562,.T.);
#14091=ADVANCED_FACE('',(#1523),#13563,.T.);
#14092=ADVANCED_FACE('',(#1524),#1314,.F.);
#14093=ADVANCED_FACE('',(#1525),#710,.F.);
#14094=ADVANCED_FACE('',(#1526,#655),#13564,.T.);
#14095=ADVANCED_FACE('',(#1527),#1315,.F.);
#14096=ADVANCED_FACE('',(#1528),#711,.F.);
#14097=ADVANCED_FACE('',(#1529,#656),#13565,.F.);
#14098=ADVANCED_FACE('',(#1530),#1316,.F.);
#14099=ADVANCED_FACE('',(#1531,#657),#13566,.F.);
#14100=ADVANCED_FACE('',(#1532),#13567,.T.);
#14101=ADVANCED_FACE('',(#1533),#13568,.T.);
#14102=ADVANCED_FACE('',(#1534),#13569,.T.);
#14103=ADVANCED_FACE('',(#1535),#13570,.T.);
#14104=ADVANCED_FACE('',(#1536),#13571,.T.);
#14105=ADVANCED_FACE('',(#1537),#13572,.T.);
#14106=ADVANCED_FACE('',(#1538),#13573,.F.);
#14107=ADVANCED_FACE('',(#1539),#13574,.F.);
#14108=ADVANCED_FACE('',(#1540),#13575,.F.);
#14109=ADVANCED_FACE('',(#1541),#1317,.F.);
#14110=ADVANCED_FACE('',(#1542,#658),#13576,.F.);
#14111=ADVANCED_FACE('',(#1543),#13577,.T.);
#14112=ADVANCED_FACE('',(#1544),#1318,.T.);
#14113=ADVANCED_FACE('',(#1545),#13578,.T.);
#14114=ADVANCED_FACE('',(#1546),#13579,.T.);
#14115=ADVANCED_FACE('',(#1547),#13580,.T.);
#14116=ADVANCED_FACE('',(#1548),#13581,.T.);
#14117=ADVANCED_FACE('',(#1549),#13582,.T.);
#14118=ADVANCED_FACE('',(#1550),#13583,.T.);
#14119=ADVANCED_FACE('',(#1551),#13584,.T.);
#14120=ADVANCED_FACE('',(#1552),#13585,.F.);
#14121=ADVANCED_FACE('',(#1553),#13586,.F.);
#14122=ADVANCED_FACE('',(#1554),#13587,.F.);
#14123=ADVANCED_FACE('',(#1555,#659),#13588,.T.);
#14124=ADVANCED_FACE('',(#1556),#13589,.T.);
#14125=ADVANCED_FACE('',(#1557),#13590,.T.);
#14126=ADVANCED_FACE('',(#1558),#13591,.T.);
#14127=ADVANCED_FACE('',(#1559),#13592,.T.);
#14128=ADVANCED_FACE('',(#1560),#13593,.T.);
#14129=ADVANCED_FACE('',(#1561),#13594,.T.);
#14130=ADVANCED_FACE('',(#1562),#13595,.T.);
#14131=ADVANCED_FACE('',(#1563),#13596,.T.);
#14132=ADVANCED_FACE('',(#1564),#13597,.T.);
#14133=ADVANCED_FACE('',(#1565),#13598,.T.);
#14134=ADVANCED_FACE('',(#1566),#13599,.T.);
#14135=ADVANCED_FACE('',(#1567),#13600,.T.);
#14136=ADVANCED_FACE('',(#1568),#13601,.T.);
#14137=ADVANCED_FACE('',(#1569),#13602,.T.);
#14138=ADVANCED_FACE('',(#1570),#13603,.T.);
#14139=ADVANCED_FACE('',(#1571),#13604,.T.);
#14140=ADVANCED_FACE('',(#1572),#13605,.T.);
#14141=ADVANCED_FACE('',(#1573),#13606,.T.);
#14142=ADVANCED_FACE('',(#1574),#13607,.T.);
#14143=ADVANCED_FACE('',(#1575),#13608,.T.);
#14144=ADVANCED_FACE('',(#1576),#13609,.T.);
#14145=ADVANCED_FACE('',(#1577),#13610,.T.);
#14146=ADVANCED_FACE('',(#1578),#13611,.T.);
#14147=ADVANCED_FACE('',(#1579),#13612,.T.);
#14148=ADVANCED_FACE('',(#1580),#13613,.T.);
#14149=ADVANCED_FACE('',(#1581),#13614,.F.);
#14150=ADVANCED_FACE('',(#1582),#13615,.F.);
#14151=ADVANCED_FACE('',(#1583),#13616,.T.);
#14152=ADVANCED_FACE('',(#1584),#13617,.T.);
#14153=ADVANCED_FACE('',(#1585,#660),#13618,.T.);
#14154=ADVANCED_FACE('',(#1586),#13619,.T.);
#14155=ADVANCED_FACE('',(#1587),#1319,.T.);
#14156=ADVANCED_FACE('',(#1588),#13620,.T.);
#14157=ADVANCED_FACE('',(#1589),#1320,.T.);
#14158=ADVANCED_FACE('',(#1590),#13621,.T.);
#14159=ADVANCED_FACE('',(#1591),#1321,.T.);
#14160=ADVANCED_FACE('',(#1592),#13622,.T.);
#14161=ADVANCED_FACE('',(#1593),#1322,.T.);
#14162=ADVANCED_FACE('',(#1594),#712,.T.);
#14163=ADVANCED_FACE('',(#1595,#661),#13623,.T.);
#14164=ADVANCED_FACE('',(#1596),#713,.T.);
#14165=ADVANCED_FACE('',(#1597),#13624,.F.);
#14166=ADVANCED_FACE('',(#1598),#13625,.T.);
#14167=ADVANCED_FACE('',(#1599),#13626,.T.);
#14168=ADVANCED_FACE('',(#1600),#13627,.T.);
#14169=ADVANCED_FACE('',(#1601),#13628,.T.);
#14170=ADVANCED_FACE('',(#1602),#1323,.T.);
#14171=ADVANCED_FACE('',(#1603),#13629,.T.);
#14172=ADVANCED_FACE('',(#1604),#1324,.T.);
#14173=ADVANCED_FACE('',(#1605),#13630,.T.);
#14174=ADVANCED_FACE('',(#1606),#1325,.T.);
#14175=ADVANCED_FACE('',(#1607),#13631,.T.);
#14176=ADVANCED_FACE('',(#1608),#1326,.T.);
#14177=ADVANCED_FACE('',(#1609),#13632,.T.);
#14178=ADVANCED_FACE('',(#1610),#13633,.T.);
#14179=ADVANCED_FACE('',(#1611),#13634,.T.);
#14180=ADVANCED_FACE('',(#1612),#13635,.T.);
#14181=ADVANCED_FACE('',(#1613),#13636,.T.);
#14182=ADVANCED_FACE('',(#1614),#13637,.T.);
#14183=ADVANCED_FACE('',(#1615),#13638,.T.);
#14184=ADVANCED_FACE('',(#1616),#714,.T.);
#14185=ADVANCED_FACE('',(#1617),#13639,.T.);
#14186=ADVANCED_FACE('',(#1618),#715,.T.);
#14187=ADVANCED_FACE('',(#1619),#13640,.T.);
#14188=ADVANCED_FACE('',(#1620),#13641,.T.);
#14189=ADVANCED_FACE('',(#1621,#662,#663),#13642,.T.);
#14190=ADVANCED_FACE('',(#1622),#13643,.T.);
#14191=ADVANCED_FACE('',(#1623),#13644,.T.);
#14192=ADVANCED_FACE('',(#1624),#105,.T.);
#14193=ADVANCED_FACE('',(#1625),#1327,.F.);
#14194=ADVANCED_FACE('',(#1626),#106,.T.);
#14195=ADVANCED_FACE('',(#1627),#107,.T.);
#14196=ADVANCED_FACE('',(#1628),#716,.F.);
#14197=ADVANCED_FACE('',(#1629),#108,.T.);
#14198=ADVANCED_FACE('',(#1630),#1328,.F.);
#14199=ADVANCED_FACE('',(#1631),#109,.T.);
#14200=ADVANCED_FACE('',(#1632),#110,.T.);
#14201=ADVANCED_FACE('',(#1633),#717,.F.);
#14202=ADVANCED_FACE('',(#1634),#1329,.F.);
#14203=ADVANCED_FACE('',(#1635),#718,.F.);
#14204=ADVANCED_FACE('',(#1636),#1330,.F.);
#14205=ADVANCED_FACE('',(#1637,#664),#13645,.F.);
#14206=ADVANCED_FACE('',(#1638),#13646,.T.);
#14207=ADVANCED_FACE('',(#1639),#13647,.T.);
#14208=ADVANCED_FACE('',(#1640),#13648,.F.);
#14209=ADVANCED_FACE('',(#1641),#13649,.F.);
#14210=ADVANCED_FACE('',(#1642),#13650,.F.);
#14211=ADVANCED_FACE('',(#1643),#13651,.F.);
#14212=ADVANCED_FACE('',(#1644),#13652,.F.);
#14213=ADVANCED_FACE('',(#1645),#13653,.F.);
#14214=ADVANCED_FACE('',(#1646),#13654,.F.);
#14215=ADVANCED_FACE('',(#1647),#13655,.F.);
#14216=ADVANCED_FACE('',(#1648),#13656,.T.);
#14217=ADVANCED_FACE('',(#1649),#1331,.F.);
#14218=ADVANCED_FACE('',(#1650),#719,.F.);
#14219=ADVANCED_FACE('',(#1651,#665,#666,#667),#13657,.F.);
#14220=ADVANCED_FACE('',(#1652),#1332,.F.);
#14221=ADVANCED_FACE('',(#1653,#668,#669,#670),#13658,.T.);
#14222=ADVANCED_FACE('',(#1654),#13659,.T.);
#14223=ADVANCED_FACE('',(#1655),#1333,.T.);
#14224=ADVANCED_FACE('',(#1656),#13660,.T.);
#14225=ADVANCED_FACE('',(#1657),#1334,.T.);
#14226=ADVANCED_FACE('',(#1658),#13661,.T.);
#14227=ADVANCED_FACE('',(#1659),#1335,.T.);
#14228=ADVANCED_FACE('',(#1660),#13662,.T.);
#14229=ADVANCED_FACE('',(#1661),#1336,.T.);
#14230=ADVANCED_FACE('',(#1662),#720,.T.);
#14231=ADVANCED_FACE('',(#1663),#13663,.T.);
#14232=ADVANCED_FACE('',(#1664),#721,.T.);
#14233=ADVANCED_FACE('',(#1665),#13664,.T.);
#14234=ADVANCED_FACE('',(#1666),#13665,.T.);
#14235=ADVANCED_FACE('',(#1667),#1337,.T.);
#14236=ADVANCED_FACE('',(#1668),#13666,.T.);
#14237=ADVANCED_FACE('',(#1669),#1338,.T.);
#14238=ADVANCED_FACE('',(#1670),#13667,.T.);
#14239=ADVANCED_FACE('',(#1671),#1339,.T.);
#14240=ADVANCED_FACE('',(#1672),#13668,.T.);
#14241=ADVANCED_FACE('',(#1673),#1340,.T.);
#14242=ADVANCED_FACE('',(#1674),#1341,.T.);
#14243=ADVANCED_FACE('',(#1675),#13669,.T.);
#14244=ADVANCED_FACE('',(#1676),#1342,.T.);
#14245=ADVANCED_FACE('',(#1677),#13670,.T.);
#14246=ADVANCED_FACE('',(#1678),#13671,.T.);
#14247=ADVANCED_FACE('',(#1679),#13672,.T.);
#14248=ADVANCED_FACE('',(#1680),#1343,.T.);
#14249=ADVANCED_FACE('',(#1681),#13673,.T.);
#14250=ADVANCED_FACE('',(#1682),#1344,.T.);
#14251=ADVANCED_FACE('',(#1683),#13674,.T.);
#14252=ADVANCED_FACE('',(#1684),#1345,.T.);
#14253=ADVANCED_FACE('',(#1685),#13675,.T.);
#14254=ADVANCED_FACE('',(#1686),#1346,.T.);
#14255=ADVANCED_FACE('',(#1687),#1347,.T.);
#14256=ADVANCED_FACE('',(#1688),#13676,.T.);
#14257=ADVANCED_FACE('',(#1689),#1348,.T.);
#14258=ADVANCED_FACE('',(#1690),#13677,.T.);
#14259=ADVANCED_FACE('',(#1691),#722,.F.);
#14260=ADVANCED_FACE('',(#1692),#723,.F.);
#14261=ADVANCED_FACE('',(#1693),#724,.T.);
#14262=ADVANCED_FACE('',(#1694),#725,.T.);
#14263=ADVANCED_FACE('',(#1695),#13678,.T.);
#14264=ADVANCED_FACE('',(#1696),#13679,.T.);
#14265=ADVANCED_FACE('',(#1697),#13680,.T.);
#14266=ADVANCED_FACE('',(#1698),#13681,.T.);
#14267=ADVANCED_FACE('',(#1699),#13682,.T.);
#14268=ADVANCED_FACE('',(#1700),#13683,.T.);
#14269=ADVANCED_FACE('',(#1701),#13684,.T.);
#14270=ADVANCED_FACE('',(#1702),#13685,.T.);
#14271=ADVANCED_FACE('',(#1703),#13686,.T.);
#14272=ADVANCED_FACE('',(#1704),#13687,.T.);
#14273=ADVANCED_FACE('',(#1705),#13688,.T.);
#14274=ADVANCED_FACE('',(#1706),#13689,.T.);
#14275=ADVANCED_FACE('',(#1707),#13690,.T.);
#14276=ADVANCED_FACE('',(#1708),#13691,.T.);
#14277=ADVANCED_FACE('',(#1709),#13692,.T.);
#14278=ADVANCED_FACE('',(#1710),#13693,.T.);
#14279=ADVANCED_FACE('',(#1711),#13694,.T.);
#14280=ADVANCED_FACE('',(#1712),#13695,.T.);
#14281=ADVANCED_FACE('',(#1713),#13696,.T.);
#14282=ADVANCED_FACE('',(#1714),#13697,.T.);
#14283=ADVANCED_FACE('',(#1715,#671,#672,#673),#13698,.T.);
#14284=ADVANCED_FACE('',(#1716),#13699,.F.);
#14285=ADVANCED_FACE('',(#1717),#13700,.T.);
#14286=ADVANCED_FACE('',(#1718),#13701,.T.);
#14287=ADVANCED_FACE('',(#1719),#13702,.T.);
#14288=ADVANCED_FACE('',(#1720),#13703,.T.);
#14289=ADVANCED_FACE('',(#1721),#13704,.T.);
#14290=ADVANCED_FACE('',(#1722),#13705,.T.);
#14291=ADVANCED_FACE('',(#1723),#13706,.T.);
#14292=ADVANCED_FACE('',(#1724),#13707,.T.);
#14293=ADVANCED_FACE('',(#1725),#13708,.T.);
#14294=ADVANCED_FACE('',(#1726),#13709,.T.);
#14295=ADVANCED_FACE('',(#1727),#13710,.T.);
#14296=ADVANCED_FACE('',(#1728),#13711,.T.);
#14297=ADVANCED_FACE('',(#1729),#13712,.T.);
#14298=ADVANCED_FACE('',(#1730),#13713,.T.);
#14299=ADVANCED_FACE('',(#1731),#13714,.T.);
#14300=ADVANCED_FACE('',(#1732),#13715,.T.);
#14301=ADVANCED_FACE('',(#1733),#13716,.T.);
#14302=ADVANCED_FACE('',(#1734),#13717,.T.);
#14303=ADVANCED_FACE('',(#1735),#13718,.T.);
#14304=ADVANCED_FACE('',(#1736),#13719,.T.);
#14305=ADVANCED_FACE('',(#1737),#13720,.T.);
#14306=ADVANCED_FACE('',(#1738),#13721,.T.);
#14307=ADVANCED_FACE('',(#1739,#674),#13722,.F.);
#14308=ADVANCED_FACE('',(#1740),#13723,.T.);
#14309=ADVANCED_FACE('',(#1741,#675),#13724,.T.);
#14310=ADVANCED_FACE('',(#1742),#13725,.T.);
#14311=ADVANCED_FACE('',(#1743),#726,.F.);
#14312=ADVANCED_FACE('',(#1744),#727,.T.);
#14313=ADVANCED_FACE('',(#1745),#728,.T.);
#14314=ADVANCED_FACE('',(#1746),#729,.T.);
#14315=ADVANCED_FACE('',(#1747),#730,.T.);
#14316=ADVANCED_FACE('',(#1748),#731,.T.);
#14317=ADVANCED_FACE('',(#1749),#732,.T.);
#14318=ADVANCED_FACE('',(#1750),#733,.T.);
#14319=ADVANCED_FACE('',(#1751),#734,.T.);
#14320=ADVANCED_FACE('',(#1752),#735,.T.);
#14321=ADVANCED_FACE('',(#1753),#736,.T.);
#14322=ADVANCED_FACE('',(#1754),#737,.T.);
#14323=ADVANCED_FACE('',(#1755),#738,.T.);
#14324=ADVANCED_FACE('',(#1756),#739,.T.);
#14325=ADVANCED_FACE('',(#1757),#740,.T.);
#14326=ADVANCED_FACE('',(#1758),#741,.T.);
#14327=ADVANCED_FACE('',(#1759),#742,.T.);
#14328=ADVANCED_FACE('',(#1760),#743,.T.);
#14329=ADVANCED_FACE('',(#1761),#744,.T.);
#14330=ADVANCED_FACE('',(#1762),#745,.T.);
#14331=ADVANCED_FACE('',(#1763),#746,.T.);
#14332=ADVANCED_FACE('',(#1764),#747,.T.);
#14333=ADVANCED_FACE('',(#1765),#748,.T.);
#14334=ADVANCED_FACE('',(#1766),#749,.T.);
#14335=ADVANCED_FACE('',(#1767),#750,.T.);
#14336=ADVANCED_FACE('',(#1768),#751,.T.);
#14337=ADVANCED_FACE('',(#1769),#752,.T.);
#14338=ADVANCED_FACE('',(#1770),#753,.T.);
#14339=ADVANCED_FACE('',(#1771),#754,.T.);
#14340=ADVANCED_FACE('',(#1772),#755,.T.);
#14341=ADVANCED_FACE('',(#1773),#756,.T.);
#14342=ADVANCED_FACE('',(#1774),#757,.T.);
#14343=ADVANCED_FACE('',(#1775),#758,.T.);
#14344=ADVANCED_FACE('',(#1776),#759,.T.);
#14345=ADVANCED_FACE('',(#1777),#760,.T.);
#14346=ADVANCED_FACE('',(#1778),#761,.T.);
#14347=ADVANCED_FACE('',(#1779),#762,.T.);
#14348=ADVANCED_FACE('',(#1780),#763,.T.);
#14349=ADVANCED_FACE('',(#1781),#764,.T.);
#14350=ADVANCED_FACE('',(#1782),#765,.T.);
#14351=ADVANCED_FACE('',(#1783),#766,.T.);
#14352=ADVANCED_FACE('',(#1784),#767,.T.);
#14353=ADVANCED_FACE('',(#1785),#768,.T.);
#14354=ADVANCED_FACE('',(#1786),#769,.T.);
#14355=ADVANCED_FACE('',(#1787),#770,.T.);
#14356=ADVANCED_FACE('',(#1788),#771,.T.);
#14357=ADVANCED_FACE('',(#1789),#772,.T.);
#14358=ADVANCED_FACE('',(#1790),#773,.T.);
#14359=ADVANCED_FACE('',(#1791),#774,.T.);
#14360=ADVANCED_FACE('',(#1792),#775,.T.);
#14361=ADVANCED_FACE('',(#1793),#776,.T.);
#14362=ADVANCED_FACE('',(#1794),#777,.T.);
#14363=ADVANCED_FACE('',(#1795),#778,.T.);
#14364=ADVANCED_FACE('',(#1796),#779,.T.);
#14365=ADVANCED_FACE('',(#1797),#780,.T.);
#14366=ADVANCED_FACE('',(#1798),#781,.T.);
#14367=ADVANCED_FACE('',(#1799),#1349,.T.);
#14368=ADVANCED_FACE('',(#1800),#782,.T.);
#14369=ADVANCED_FACE('',(#1801,#676),#13726,.T.);
#14370=ADVANCED_FACE('',(#1802),#111,.F.);
#14371=ADVANCED_FACE('',(#1803),#13727,.T.);
#14372=ADVANCED_FACE('',(#1804),#783,.T.);
#14373=ADVANCED_FACE('',(#1805),#112,.F.);
#14374=ADVANCED_FACE('',(#1806),#13728,.F.);
#14375=ADVANCED_FACE('',(#1807),#13729,.T.);
#14376=ADVANCED_FACE('',(#1808),#13730,.F.);
#14377=ADVANCED_FACE('',(#1809),#13731,.F.);
#14378=ADVANCED_FACE('',(#1810),#13732,.F.);
#14379=ADVANCED_FACE('',(#1811),#13733,.T.);
#14380=ADVANCED_FACE('',(#1812),#13734,.F.);
#14381=ADVANCED_FACE('',(#1813),#13735,.F.);
#14382=ADVANCED_FACE('',(#1814),#13736,.F.);
#14383=ADVANCED_FACE('',(#1815),#13737,.T.);
#14384=ADVANCED_FACE('',(#1816),#13738,.F.);
#14385=ADVANCED_FACE('',(#1817),#13739,.F.);
#14386=ADVANCED_FACE('',(#1818),#13740,.F.);
#14387=ADVANCED_FACE('',(#1819),#13741,.T.);
#14388=ADVANCED_FACE('',(#1820),#13742,.F.);
#14389=ADVANCED_FACE('',(#1821),#13743,.F.);
#14390=ADVANCED_FACE('',(#1822),#13744,.F.);
#14391=ADVANCED_FACE('',(#1823),#13745,.T.);
#14392=ADVANCED_FACE('',(#1824),#13746,.F.);
#14393=ADVANCED_FACE('',(#1825),#13747,.F.);
#14394=ADVANCED_FACE('',(#1826),#13748,.F.);
#14395=ADVANCED_FACE('',(#1827),#13749,.T.);
#14396=ADVANCED_FACE('',(#1828),#13750,.F.);
#14397=ADVANCED_FACE('',(#1829),#13751,.F.);
#14398=ADVANCED_FACE('',(#1830),#13752,.F.);
#14399=ADVANCED_FACE('',(#1831),#13753,.T.);
#14400=ADVANCED_FACE('',(#1832),#13754,.F.);
#14401=ADVANCED_FACE('',(#1833),#13755,.F.);
#14402=ADVANCED_FACE('',(#1834),#13756,.F.);
#14403=ADVANCED_FACE('',(#1835),#13757,.T.);
#14404=ADVANCED_FACE('',(#1836),#13758,.F.);
#14405=ADVANCED_FACE('',(#1837),#13759,.F.);
#14406=ADVANCED_FACE('',(#1838),#13760,.F.);
#14407=ADVANCED_FACE('',(#1839),#13761,.T.);
#14408=ADVANCED_FACE('',(#1840),#13762,.F.);
#14409=ADVANCED_FACE('',(#1841),#13763,.F.);
#14410=ADVANCED_FACE('',(#1842),#13764,.F.);
#14411=ADVANCED_FACE('',(#1843),#13765,.T.);
#14412=ADVANCED_FACE('',(#1844),#13766,.F.);
#14413=ADVANCED_FACE('',(#1845),#13767,.F.);
#14414=ADVANCED_FACE('',(#1846),#13768,.F.);
#14415=ADVANCED_FACE('',(#1847),#13769,.T.);
#14416=ADVANCED_FACE('',(#1848),#13770,.F.);
#14417=ADVANCED_FACE('',(#1849),#13771,.F.);
#14418=ADVANCED_FACE('',(#1850),#13772,.F.);
#14419=ADVANCED_FACE('',(#1851),#13773,.T.);
#14420=ADVANCED_FACE('',(#1852),#13774,.F.);
#14421=ADVANCED_FACE('',(#1853),#13775,.F.);
#14422=ADVANCED_FACE('',(#1854),#13776,.F.);
#14423=ADVANCED_FACE('',(#1855),#13777,.T.);
#14424=ADVANCED_FACE('',(#1856),#13778,.F.);
#14425=ADVANCED_FACE('',(#1857),#13779,.F.);
#14426=ADVANCED_FACE('',(#1858),#13780,.F.);
#14427=ADVANCED_FACE('',(#1859),#13781,.T.);
#14428=ADVANCED_FACE('',(#1860),#13782,.F.);
#14429=ADVANCED_FACE('',(#1861),#13783,.F.);
#14430=ADVANCED_FACE('',(#1862),#13784,.F.);
#14431=ADVANCED_FACE('',(#1863),#13785,.T.);
#14432=ADVANCED_FACE('',(#1864),#13786,.F.);
#14433=ADVANCED_FACE('',(#1865),#13787,.F.);
#14434=ADVANCED_FACE('',(#1866),#13788,.F.);
#14435=ADVANCED_FACE('',(#1867),#13789,.T.);
#14436=ADVANCED_FACE('',(#1868),#13790,.F.);
#14437=ADVANCED_FACE('',(#1869),#13791,.F.);
#14438=ADVANCED_FACE('',(#1870),#13792,.F.);
#14439=ADVANCED_FACE('',(#1871),#13793,.T.);
#14440=ADVANCED_FACE('',(#1872),#13794,.F.);
#14441=ADVANCED_FACE('',(#1873),#13795,.F.);
#14442=ADVANCED_FACE('',(#1874),#13796,.F.);
#14443=ADVANCED_FACE('',(#1875),#13797,.T.);
#14444=ADVANCED_FACE('',(#1876),#13798,.F.);
#14445=ADVANCED_FACE('',(#1877),#13799,.F.);
#14446=ADVANCED_FACE('',(#1878),#13800,.F.);
#14447=ADVANCED_FACE('',(#1879),#13801,.T.);
#14448=ADVANCED_FACE('',(#1880),#13802,.F.);
#14449=ADVANCED_FACE('',(#1881),#13803,.F.);
#14450=ADVANCED_FACE('',(#1882),#13804,.F.);
#14451=ADVANCED_FACE('',(#1883),#13805,.T.);
#14452=ADVANCED_FACE('',(#1884),#13806,.F.);
#14453=ADVANCED_FACE('',(#1885),#13807,.F.);
#14454=ADVANCED_FACE('',(#1886),#13808,.F.);
#14455=ADVANCED_FACE('',(#1887),#13809,.T.);
#14456=ADVANCED_FACE('',(#1888),#13810,.F.);
#14457=ADVANCED_FACE('',(#1889),#13811,.F.);
#14458=ADVANCED_FACE('',(#1890),#13812,.F.);
#14459=ADVANCED_FACE('',(#1891),#13813,.T.);
#14460=ADVANCED_FACE('',(#1892),#13814,.F.);
#14461=ADVANCED_FACE('',(#1893),#13815,.F.);
#14462=ADVANCED_FACE('',(#1894),#13816,.F.);
#14463=ADVANCED_FACE('',(#1895),#13817,.T.);
#14464=ADVANCED_FACE('',(#1896),#13818,.F.);
#14465=ADVANCED_FACE('',(#1897),#13819,.F.);
#14466=ADVANCED_FACE('',(#1898),#13820,.F.);
#14467=ADVANCED_FACE('',(#1899),#13821,.T.);
#14468=ADVANCED_FACE('',(#1900),#13822,.F.);
#14469=ADVANCED_FACE('',(#1901),#13823,.F.);
#14470=ADVANCED_FACE('',(#1902),#13824,.T.);
#14471=ADVANCED_FACE('',(#1903),#1350,.T.);
#14472=ADVANCED_FACE('',(#1904),#784,.T.);
#14473=ADVANCED_FACE('',(#1905),#1351,.T.);
#14474=ADVANCED_FACE('',(#1906,#677),#13825,.T.);
#14475=ADVANCED_FACE('',(#1907),#785,.F.);
#14476=ADVANCED_FACE('',(#1908),#13826,.T.);
#14477=ADVANCED_FACE('',(#1909),#1352,.F.);
#14478=ADVANCED_FACE('',(#1910),#786,.F.);
#14479=ADVANCED_FACE('',(#1911,#678),#13827,.T.);
#14480=ADVANCED_FACE('',(#1912),#13828,.T.);
#14481=ADVANCED_FACE('',(#1913),#787,.T.);
#14482=ADVANCED_FACE('',(#1914),#1353,.T.);
#14483=ADVANCED_FACE('',(#1915),#13829,.T.);
#14484=ADVANCED_FACE('',(#1916),#13830,.T.);
#14485=ADVANCED_FACE('',(#1917),#13831,.T.);
#14486=ADVANCED_FACE('',(#1918),#13832,.T.);
#14487=ADVANCED_FACE('',(#1919),#13833,.T.);
#14488=ADVANCED_FACE('',(#1920),#13834,.T.);
#14489=ADVANCED_FACE('',(#1921),#13835,.T.);
#14490=ADVANCED_FACE('',(#1922),#13836,.T.);
#14491=ADVANCED_FACE('',(#1923),#13837,.T.);
#14492=ADVANCED_FACE('',(#1924),#13838,.T.);
#14493=ADVANCED_FACE('',(#1925),#13839,.T.);
#14494=ADVANCED_FACE('',(#1926),#13840,.T.);
#14495=ADVANCED_FACE('',(#1927),#13841,.T.);
#14496=ADVANCED_FACE('',(#1928),#13842,.T.);
#14497=ADVANCED_FACE('',(#1929),#13843,.T.);
#14498=ADVANCED_FACE('',(#1930),#13844,.T.);
#14499=ADVANCED_FACE('',(#1931),#13845,.T.);
#14500=ADVANCED_FACE('',(#1932),#13846,.T.);
#14501=ADVANCED_FACE('',(#1933),#13847,.T.);
#14502=ADVANCED_FACE('',(#1934),#13848,.T.);
#14503=ADVANCED_FACE('',(#1935),#13849,.T.);
#14504=ADVANCED_FACE('',(#1936),#13850,.T.);
#14505=ADVANCED_FACE('',(#1937),#13851,.T.);
#14506=ADVANCED_FACE('',(#1938),#13852,.T.);
#14507=ADVANCED_FACE('',(#1939),#13853,.T.);
#14508=ADVANCED_FACE('',(#1940),#13854,.T.);
#14509=ADVANCED_FACE('',(#1941),#13855,.T.);
#14510=ADVANCED_FACE('',(#1942),#13856,.T.);
#14511=ADVANCED_FACE('',(#1943),#13857,.T.);
#14512=ADVANCED_FACE('',(#1944),#113,.T.);
#14513=ADVANCED_FACE('',(#1945),#13858,.T.);
#14514=ADVANCED_FACE('',(#1946),#13859,.T.);
#14515=ADVANCED_FACE('',(#1947),#788,.F.);
#14516=ADVANCED_FACE('',(#1948),#1354,.F.);
#14517=ADVANCED_FACE('',(#1949,#679),#13860,.F.);
#14518=ADVANCED_FACE('',(#1950),#13861,.T.);
#14519=ADVANCED_FACE('',(#1951),#13862,.T.);
#14520=ADVANCED_FACE('',(#1952),#13863,.T.);
#14521=ADVANCED_FACE('',(#1953),#13864,.T.);
#14522=ADVANCED_FACE('',(#1954),#13865,.T.);
#14523=ADVANCED_FACE('',(#1955),#13866,.T.);
#14524=ADVANCED_FACE('',(#1956),#13867,.F.);
#14525=ADVANCED_FACE('',(#1957),#13868,.F.);
#14526=ADVANCED_FACE('',(#1958),#13869,.F.);
#14527=ADVANCED_FACE('',(#1959,#680),#13870,.T.);
#14528=ADVANCED_FACE('',(#1960),#13871,.F.);
#14529=ADVANCED_FACE('',(#1961),#13872,.F.);
#14530=ADVANCED_FACE('',(#1962),#13873,.F.);
#14531=ADVANCED_FACE('',(#1963),#13874,.T.);
#14532=ADVANCED_FACE('',(#1964),#789,.F.);
#14533=ADVANCED_FACE('',(#1965),#13875,.T.);
#14534=ADVANCED_FACE('',(#1966),#13876,.T.);
#14535=ADVANCED_FACE('',(#1967),#790,.F.);
#14536=ADVANCED_FACE('',(#1968),#791,.F.);
#14537=ADVANCED_FACE('',(#1969),#13877,.T.);
#14538=ADVANCED_FACE('',(#1970),#13878,.T.);
#14539=ADVANCED_FACE('',(#1971),#792,.F.);
#14540=ADVANCED_FACE('',(#1972),#793,.F.);
#14541=ADVANCED_FACE('',(#1973),#13879,.T.);
#14542=ADVANCED_FACE('',(#1974),#13880,.T.);
#14543=ADVANCED_FACE('',(#1975),#794,.F.);
#14544=ADVANCED_FACE('',(#1976),#795,.F.);
#14545=ADVANCED_FACE('',(#1977),#13881,.T.);
#14546=ADVANCED_FACE('',(#1978),#13882,.T.);
#14547=ADVANCED_FACE('',(#1979),#796,.F.);
#14548=ADVANCED_FACE('',(#1980),#797,.F.);
#14549=ADVANCED_FACE('',(#1981),#13883,.T.);
#14550=ADVANCED_FACE('',(#1982),#13884,.T.);
#14551=ADVANCED_FACE('',(#1983),#798,.F.);
#14552=ADVANCED_FACE('',(#1984),#799,.F.);
#14553=ADVANCED_FACE('',(#1985),#13885,.T.);
#14554=ADVANCED_FACE('',(#1986),#13886,.T.);
#14555=ADVANCED_FACE('',(#1987),#800,.F.);
#14556=ADVANCED_FACE('',(#1988),#801,.F.);
#14557=ADVANCED_FACE('',(#1989),#13887,.T.);
#14558=ADVANCED_FACE('',(#1990),#13888,.T.);
#14559=ADVANCED_FACE('',(#1991),#802,.F.);
#14560=ADVANCED_FACE('',(#1992),#803,.F.);
#14561=ADVANCED_FACE('',(#1993),#13889,.T.);
#14562=ADVANCED_FACE('',(#1994),#1355,.T.);
#14563=ADVANCED_FACE('',(#1995),#804,.T.);
#14564=ADVANCED_FACE('',(#1996),#805,.T.);
#14565=ADVANCED_FACE('',(#1997),#806,.T.);
#14566=ADVANCED_FACE('',(#1998),#807,.T.);
#14567=ADVANCED_FACE('',(#1999),#808,.T.);
#14568=ADVANCED_FACE('',(#2000),#809,.T.);
#14569=ADVANCED_FACE('',(#2001),#810,.T.);
#14570=ADVANCED_FACE('',(#2002),#811,.T.);
#14571=ADVANCED_FACE('',(#2003),#812,.T.);
#14572=ADVANCED_FACE('',(#2004),#813,.T.);
#14573=ADVANCED_FACE('',(#2005),#814,.T.);
#14574=ADVANCED_FACE('',(#2006),#815,.T.);
#14575=ADVANCED_FACE('',(#2007),#816,.T.);
#14576=ADVANCED_FACE('',(#2008),#817,.T.);
#14577=ADVANCED_FACE('',(#2009),#818,.T.);
#14578=ADVANCED_FACE('',(#2010),#819,.T.);
#14579=ADVANCED_FACE('',(#2011),#820,.T.);
#14580=ADVANCED_FACE('',(#2012),#821,.T.);
#14581=ADVANCED_FACE('',(#2013),#822,.T.);
#14582=ADVANCED_FACE('',(#2014),#823,.T.);
#14583=ADVANCED_FACE('',(#2015),#824,.T.);
#14584=ADVANCED_FACE('',(#2016),#825,.T.);
#14585=ADVANCED_FACE('',(#2017),#826,.T.);
#14586=ADVANCED_FACE('',(#2018),#827,.T.);
#14587=ADVANCED_FACE('',(#2019),#828,.T.);
#14588=ADVANCED_FACE('',(#2020),#829,.T.);
#14589=ADVANCED_FACE('',(#2021),#830,.T.);
#14590=ADVANCED_FACE('',(#2022),#831,.T.);
#14591=ADVANCED_FACE('',(#2023),#832,.T.);
#14592=ADVANCED_FACE('',(#2024),#833,.T.);
#14593=ADVANCED_FACE('',(#2025),#834,.T.);
#14594=ADVANCED_FACE('',(#2026),#835,.T.);
#14595=ADVANCED_FACE('',(#2027),#836,.T.);
#14596=ADVANCED_FACE('',(#2028),#837,.T.);
#14597=ADVANCED_FACE('',(#2029),#838,.T.);
#14598=ADVANCED_FACE('',(#2030),#839,.T.);
#14599=ADVANCED_FACE('',(#2031),#840,.T.);
#14600=ADVANCED_FACE('',(#2032),#841,.T.);
#14601=ADVANCED_FACE('',(#2033),#842,.T.);
#14602=ADVANCED_FACE('',(#2034),#843,.T.);
#14603=ADVANCED_FACE('',(#2035),#844,.T.);
#14604=ADVANCED_FACE('',(#2036),#845,.T.);
#14605=ADVANCED_FACE('',(#2037),#846,.T.);
#14606=ADVANCED_FACE('',(#2038),#847,.T.);
#14607=ADVANCED_FACE('',(#2039),#848,.T.);
#14608=ADVANCED_FACE('',(#2040),#114,.F.);
#14609=ADVANCED_FACE('',(#2041),#13890,.T.);
#14610=ADVANCED_FACE('',(#2042),#849,.T.);
#14611=ADVANCED_FACE('',(#2043),#115,.F.);
#14612=ADVANCED_FACE('',(#2044),#850,.T.);
#14613=ADVANCED_FACE('',(#2045),#13891,.T.);
#14614=ADVANCED_FACE('',(#2046),#1356,.T.);
#14615=ADVANCED_FACE('',(#2047),#1357,.T.);
#14616=ADVANCED_FACE('',(#2048),#13892,.T.);
#14617=ADVANCED_FACE('',(#2049),#13893,.T.);
#14618=ADVANCED_FACE('',(#2050),#13894,.T.);
#14619=ADVANCED_FACE('',(#2051),#13895,.T.);
#14620=ADVANCED_FACE('',(#2052),#13896,.T.);
#14621=ADVANCED_FACE('',(#2053),#13897,.T.);
#14622=ADVANCED_FACE('',(#2054),#13898,.T.);
#14623=ADVANCED_FACE('',(#2055,#681),#13899,.F.);
#14624=ADVANCED_FACE('',(#2056),#851,.T.);
#14625=ADVANCED_FACE('',(#2057),#852,.T.);
#14626=ADVANCED_FACE('',(#2058),#853,.T.);
#14627=ADVANCED_FACE('',(#2059),#854,.T.);
#14628=ADVANCED_FACE('',(#2060),#855,.T.);
#14629=ADVANCED_FACE('',(#2061),#856,.T.);
#14630=ADVANCED_FACE('',(#2062),#857,.T.);
#14631=ADVANCED_FACE('',(#2063),#858,.T.);
#14632=ADVANCED_FACE('',(#2064),#859,.T.);
#14633=ADVANCED_FACE('',(#2065),#860,.T.);
#14634=ADVANCED_FACE('',(#2066),#861,.T.);
#14635=ADVANCED_FACE('',(#2067),#862,.T.);
#14636=ADVANCED_FACE('',(#2068),#863,.T.);
#14637=ADVANCED_FACE('',(#2069),#864,.T.);
#14638=ADVANCED_FACE('',(#2070),#865,.T.);
#14639=ADVANCED_FACE('',(#2071),#866,.T.);
#14640=ADVANCED_FACE('',(#2072),#867,.T.);
#14641=ADVANCED_FACE('',(#2073),#868,.T.);
#14642=ADVANCED_FACE('',(#2074),#869,.T.);
#14643=ADVANCED_FACE('',(#2075),#870,.T.);
#14644=ADVANCED_FACE('',(#2076),#871,.T.);
#14645=ADVANCED_FACE('',(#2077),#872,.T.);
#14646=ADVANCED_FACE('',(#2078),#873,.T.);
#14647=ADVANCED_FACE('',(#2079),#874,.T.);
#14648=ADVANCED_FACE('',(#2080),#875,.T.);
#14649=ADVANCED_FACE('',(#2081),#876,.T.);
#14650=ADVANCED_FACE('',(#2082),#877,.T.);
#14651=ADVANCED_FACE('',(#2083),#878,.T.);
#14652=ADVANCED_FACE('',(#2084),#879,.T.);
#14653=ADVANCED_FACE('',(#2085),#880,.T.);
#14654=ADVANCED_FACE('',(#2086),#881,.T.);
#14655=ADVANCED_FACE('',(#2087),#882,.T.);
#14656=ADVANCED_FACE('',(#2088),#883,.T.);
#14657=ADVANCED_FACE('',(#2089),#884,.T.);
#14658=ADVANCED_FACE('',(#2090),#885,.T.);
#14659=ADVANCED_FACE('',(#2091),#886,.T.);
#14660=ADVANCED_FACE('',(#2092),#887,.T.);
#14661=ADVANCED_FACE('',(#2093),#888,.T.);
#14662=ADVANCED_FACE('',(#2094),#889,.T.);
#14663=ADVANCED_FACE('',(#2095),#890,.T.);
#14664=ADVANCED_FACE('',(#2096),#891,.T.);
#14665=ADVANCED_FACE('',(#2097),#892,.T.);
#14666=ADVANCED_FACE('',(#2098),#893,.T.);
#14667=ADVANCED_FACE('',(#2099),#894,.T.);
#14668=ADVANCED_FACE('',(#2100),#895,.T.);
#14669=ADVANCED_FACE('',(#2101),#896,.T.);
#14670=ADVANCED_FACE('',(#2102),#897,.T.);
#14671=ADVANCED_FACE('',(#2103),#898,.T.);
#14672=ADVANCED_FACE('',(#2104),#899,.T.);
#14673=ADVANCED_FACE('',(#2105),#900,.T.);
#14674=ADVANCED_FACE('',(#2106),#901,.T.);
#14675=ADVANCED_FACE('',(#2107),#902,.T.);
#14676=ADVANCED_FACE('',(#2108),#903,.T.);
#14677=ADVANCED_FACE('',(#2109),#904,.T.);
#14678=ADVANCED_FACE('',(#2110),#905,.T.);
#14679=ADVANCED_FACE('',(#2111),#906,.T.);
#14680=ADVANCED_FACE('',(#2112),#116,.F.);
#14681=ADVANCED_FACE('',(#2113),#13900,.T.);
#14682=ADVANCED_FACE('',(#2114),#907,.T.);
#14683=ADVANCED_FACE('',(#2115),#117,.F.);
#14684=ADVANCED_FACE('',(#2116),#1358,.F.);
#14685=ADVANCED_FACE('',(#2117),#13901,.F.);
#14686=ADVANCED_FACE('',(#2118),#13902,.F.);
#14687=ADVANCED_FACE('',(#2119),#13903,.F.);
#14688=ADVANCED_FACE('',(#2120),#13904,.F.);
#14689=ADVANCED_FACE('',(#2121),#13905,.F.);
#14690=ADVANCED_FACE('',(#2122),#13906,.F.);
#14691=ADVANCED_FACE('',(#2123,#682),#13907,.F.);
#14692=ADVANCED_FACE('',(#2124),#13908,.T.);
#14693=ADVANCED_FACE('',(#2125),#1359,.T.);
#14694=ADVANCED_FACE('',(#2126),#908,.T.);
#14695=ADVANCED_FACE('',(#2127,#683),#13909,.T.);
#14696=ADVANCED_FACE('',(#2128),#909,.T.);
#14697=ADVANCED_FACE('',(#2129),#103,.F.);
#14698=ADVANCED_FACE('',(#2130),#1360,.T.);
#14699=ADVANCED_FACE('',(#2131),#910,.T.);
#14700=ADVANCED_FACE('',(#2132,#684),#13910,.T.);
#14701=ADVANCED_FACE('',(#2133),#911,.F.);
#14702=ADVANCED_FACE('',(#2134,#685),#13911,.T.);
#14703=ADVANCED_FACE('',(#2135),#1361,.T.);
#14704=ADVANCED_FACE('',(#2136),#13912,.T.);
#14705=ADVANCED_FACE('',(#2137),#13913,.T.);
#14706=ADVANCED_FACE('',(#2138),#1362,.T.);
#14707=ADVANCED_FACE('',(#2139),#1363,.F.);
#14708=ADVANCED_FACE('',(#2140),#912,.F.);
#14709=ADVANCED_FACE('',(#2141,#686),#13914,.F.);
#14710=ADVANCED_FACE('',(#2142),#1364,.F.);
#14711=ADVANCED_FACE('',(#2143,#687),#13915,.T.);
#14712=ADVANCED_FACE('',(#2144),#13916,.T.);
#14713=ADVANCED_FACE('',(#2145),#13917,.T.);
#14714=ADVANCED_FACE('',(#2146),#1365,.T.);
#14715=ADVANCED_FACE('',(#2147),#13918,.T.);
#14716=ADVANCED_FACE('',(#2148),#13919,.T.);
#14717=ADVANCED_FACE('',(#2149),#13920,.T.);
#14718=ADVANCED_FACE('',(#2150),#13921,.T.);
#14719=ADVANCED_FACE('',(#2151),#13922,.T.);
#14720=ADVANCED_FACE('',(#2152),#13923,.T.);
#14721=ADVANCED_FACE('',(#2153),#13924,.T.);
#14722=ADVANCED_FACE('',(#2154),#13925,.T.);
#14723=ADVANCED_FACE('',(#2155),#913,.T.);
#14724=ADVANCED_FACE('',(#2156),#914,.T.);
#14725=ADVANCED_FACE('',(#2157),#915,.T.);
#14726=ADVANCED_FACE('',(#2158),#916,.T.);
#14727=ADVANCED_FACE('',(#2159),#917,.T.);
#14728=ADVANCED_FACE('',(#2160),#918,.T.);
#14729=ADVANCED_FACE('',(#2161),#919,.T.);
#14730=ADVANCED_FACE('',(#2162),#920,.T.);
#14731=ADVANCED_FACE('',(#2163),#921,.T.);
#14732=ADVANCED_FACE('',(#2164),#922,.T.);
#14733=ADVANCED_FACE('',(#2165),#923,.T.);
#14734=ADVANCED_FACE('',(#2166),#924,.T.);
#14735=ADVANCED_FACE('',(#2167),#925,.T.);
#14736=ADVANCED_FACE('',(#2168),#926,.T.);
#14737=ADVANCED_FACE('',(#2169),#927,.T.);
#14738=ADVANCED_FACE('',(#2170),#928,.T.);
#14739=ADVANCED_FACE('',(#2171),#929,.T.);
#14740=ADVANCED_FACE('',(#2172),#930,.T.);
#14741=ADVANCED_FACE('',(#2173),#931,.T.);
#14742=ADVANCED_FACE('',(#2174),#932,.T.);
#14743=ADVANCED_FACE('',(#2175),#933,.T.);
#14744=ADVANCED_FACE('',(#2176),#934,.T.);
#14745=ADVANCED_FACE('',(#2177),#935,.T.);
#14746=ADVANCED_FACE('',(#2178),#936,.T.);
#14747=ADVANCED_FACE('',(#2179),#937,.T.);
#14748=ADVANCED_FACE('',(#2180),#938,.T.);
#14749=ADVANCED_FACE('',(#2181),#939,.T.);
#14750=ADVANCED_FACE('',(#2182),#940,.T.);
#14751=ADVANCED_FACE('',(#2183),#941,.T.);
#14752=ADVANCED_FACE('',(#2184),#942,.T.);
#14753=ADVANCED_FACE('',(#2185),#943,.T.);
#14754=ADVANCED_FACE('',(#2186),#944,.T.);
#14755=ADVANCED_FACE('',(#2187),#945,.T.);
#14756=ADVANCED_FACE('',(#2188),#946,.T.);
#14757=ADVANCED_FACE('',(#2189),#947,.T.);
#14758=ADVANCED_FACE('',(#2190),#118,.F.);
#14759=ADVANCED_FACE('',(#2191),#13926,.T.);
#14760=ADVANCED_FACE('',(#2192),#948,.T.);
#14761=ADVANCED_FACE('',(#2193),#119,.F.);
#14762=ADVANCED_FACE('',(#2194),#1366,.F.);
#14763=ADVANCED_FACE('',(#2195),#13927,.F.);
#14764=ADVANCED_FACE('',(#2196),#13928,.F.);
#14765=ADVANCED_FACE('',(#2197),#13929,.F.);
#14766=ADVANCED_FACE('',(#2198),#13930,.F.);
#14767=ADVANCED_FACE('',(#2199),#13931,.F.);
#14768=ADVANCED_FACE('',(#2200),#13932,.F.);
#14769=ADVANCED_FACE('',(#2201,#688),#13933,.F.);
#14770=ADVANCED_FACE('',(#2202),#13934,.T.);
#14771=ADVANCED_FACE('',(#2203),#1367,.T.);
#14772=ADVANCED_FACE('',(#2204),#949,.T.);
#14773=ADVANCED_FACE('',(#2205,#689),#13935,.T.);
#14774=ADVANCED_FACE('',(#2206),#950,.T.);
#14775=ADVANCED_FACE('',(#2207),#104,.F.);
#14776=CLOSED_SHELL('',(#13936,#13937,#13938,#13939,#13940,#13941,#13942,
#13943,#13944,#13945,#13946,#13947,#13948,#13949,#13950,#13951,#13952,#13953,
#13954,#13955,#13956,#13957,#13958,#13959,#13960,#13961,#13962,#13963,#13964,
#13965,#13966,#13967,#13968,#13969,#13970,#13971,#13972,#13973,#13974,#13975,
#13976,#13977));
#14777=CLOSED_SHELL('',(#13978,#13979,#13980,#13981,#13982,#13983,#13984,
#13985,#13986,#13987,#13988,#13989,#13990,#13991,#13992,#13993,#13994,#13995,
#13996,#13997,#13998,#13999,#14000,#14001,#14002,#14003,#14004,#14005,#14006,
#14007,#14008,#14009,#14010,#14011,#14012,#14013,#14014,#14015,#14016,#14017,
#14018,#14019,#14020,#14021,#14022,#14023,#14024,#14025,#14026,#14027,#14028,
#14029,#14030,#14031,#14032,#14033,#14034,#14035,#14036,#14037,#14038,#14039,
#14040,#14041,#14042,#14043,#14044,#14045,#14046,#14047,#14048,#14049,#14050,
#14051,#14052,#14053,#14054,#14055,#14056,#14057,#14058,#14059,#14060,#14061,
#14062,#14063,#14064,#14065,#14066,#14067,#14068));
#14778=CLOSED_SHELL('',(#14069,#14070,#14071,#14072,#14073,#14074,#14075,
#14076,#14077,#14078,#14079,#14080,#14081,#14082,#14083,#14084,#14085,#14086,
#14087,#14088,#14089,#14090,#14091,#14092,#14093,#14094,#14095,#14096,#14097,
#14098,#14099,#14100,#14101,#14102,#14103,#14104,#14105,#14106,#14107,#14108,
#14109,#14110,#14111,#14112,#14113,#14114,#14115,#14116,#14117,#14118,#14119,
#14120,#14121,#14122,#14123,#14124,#14125,#14126,#14127,#14128,#14129,#14130,
#14131,#14132,#14133,#14134,#14135,#14136,#14137,#14138,#14139,#14140,#14141,
#14142,#14143,#14144,#14145,#14146,#14147,#14148,#14149,#14150,#14151,#14152,
#14153,#14154,#14155,#14156,#14157,#14158,#14159,#14160,#14161,#14162,#14163,
#14164,#14165,#14166,#14167,#14168,#14169,#14170,#14171,#14172,#14173,#14174,
#14175,#14176,#14177,#14178,#14179,#14180,#14181,#14182,#14183,#14184,#14185,
#14186,#14187,#14188,#14189,#14190,#14191,#14192,#14193,#14194,#14195,#14196,
#14197,#14198,#14199,#14200,#14201,#14202,#14203,#14204,#14205,#14206,#14207,
#14208,#14209,#14210,#14211,#14212,#14213,#14214,#14215,#14216));
#14779=CLOSED_SHELL('',(#14217,#14218,#14219,#14220,#14221,#14222,#14223,
#14224,#14225,#14226,#14227,#14228,#14229,#14230,#14231,#14232,#14233,#14234,
#14235,#14236,#14237,#14238,#14239,#14240,#14241,#14242,#14243,#14244,#14245,
#14246,#14247,#14248,#14249,#14250,#14251,#14252,#14253,#14254,#14255,#14256,
#14257,#14258,#14259,#14260,#14261,#14262,#14263));
#14780=CLOSED_SHELL('',(#14264,#14265,#14266,#14267,#14268,#14269,#14270,
#14271,#14272,#14273,#14274,#14275,#14276,#14277,#14278,#14279,#14280,#14281,
#14282,#14283,#14284));
#14781=CLOSED_SHELL('',(#14285,#14286,#14287,#14288,#14289,#14290,#14291,
#14292,#14293,#14294,#14295,#14296,#14297,#14298,#14299,#14300,#14301,#14302,
#14303,#14304,#14305,#14306,#14307,#14308,#14309,#14310,#14311));
#14782=CLOSED_SHELL('',(#14312,#14313,#14314,#14315,#14316,#14317,#14318,
#14319,#14320,#14321,#14322,#14323,#14324,#14325,#14326,#14327,#14328,#14329,
#14330,#14331,#14332,#14333,#14334,#14335,#14336,#14337,#14338,#14339,#14340,
#14341,#14342,#14343,#14344,#14345,#14346,#14347,#14348,#14349,#14350,#14351,
#14352,#14353,#14354,#14355,#14356,#14357,#14358,#14359,#14360,#14361,#14362,
#14363,#14364,#14365,#14366,#14367,#14368,#14369,#14370,#14371,#14372,#14373,
#14374,#14375,#14376,#14377,#14378,#14379,#14380,#14381,#14382,#14383,#14384,
#14385,#14386,#14387,#14388,#14389,#14390,#14391,#14392,#14393,#14394,#14395,
#14396,#14397,#14398,#14399,#14400,#14401,#14402,#14403,#14404,#14405,#14406,
#14407,#14408,#14409,#14410,#14411,#14412,#14413,#14414,#14415,#14416,#14417,
#14418,#14419,#14420,#14421,#14422,#14423,#14424,#14425,#14426,#14427,#14428,
#14429,#14430,#14431,#14432,#14433,#14434,#14435,#14436,#14437,#14438,#14439,
#14440,#14441,#14442,#14443,#14444,#14445,#14446,#14447,#14448,#14449,#14450,
#14451,#14452,#14453,#14454,#14455,#14456,#14457,#14458,#14459,#14460,#14461,
#14462,#14463,#14464,#14465,#14466,#14467,#14468,#14469,#14470,#14471,#14472,
#14473,#14474,#14475,#14476));
#14783=CLOSED_SHELL('',(#14477,#14478,#14479,#14480,#14481,#14482,#14483,
#14484,#14485,#14486,#14487,#14488,#14489,#14490,#14491,#14492,#14493,#14494,
#14495,#14496,#14497,#14498,#14499,#14500,#14501,#14502,#14503,#14504,#14505,
#14506,#14507,#14508,#14509,#14510,#14511,#14512,#14513,#14514,#14515,#14516,
#14517,#14518,#14519,#14520,#14521,#14522,#14523,#14524,#14525,#14526,#14527,
#14528,#14529,#14530,#14531,#14532,#14533,#14534,#14535,#14536,#14537,#14538,
#14539,#14540,#14541,#14542,#14543,#14544,#14545,#14546,#14547,#14548,#14549,
#14550,#14551,#14552,#14553,#14554,#14555,#14556,#14557,#14558,#14559,#14560,
#14561,#14562));
#14784=CLOSED_SHELL('',(#14563,#14564,#14565,#14566,#14567,#14568,#14569,
#14570,#14571,#14572,#14573,#14574,#14575,#14576,#14577,#14578,#14579,#14580,
#14581,#14582,#14583,#14584,#14585,#14586,#14587,#14588,#14589,#14590,#14591,
#14592,#14593,#14594,#14595,#14596,#14597,#14598,#14599,#14600,#14601,#14602,
#14603,#14604,#14605,#14606,#14607,#14608,#14609,#14610,#14611,#14612,#14613,
#14614,#14615,#14616,#14617,#14618,#14619,#14620,#14621,#14622,#14623));
#14785=CLOSED_SHELL('',(#14624,#14625,#14626,#14627,#14628,#14629,#14630,
#14631,#14632,#14633,#14634,#14635,#14636,#14637,#14638,#14639,#14640,#14641,
#14642,#14643,#14644,#14645,#14646,#14647,#14648,#14649,#14650,#14651,#14652,
#14653,#14654,#14655,#14656,#14657,#14658,#14659,#14660,#14661,#14662,#14663,
#14664,#14665,#14666,#14667,#14668,#14669,#14670,#14671,#14672,#14673,#14674,
#14675,#14676,#14677,#14678,#14679,#14680,#14681,#14682,#14683,#14684,#14685,
#14686,#14687,#14688,#14689,#14690,#14691,#14692,#14693,#14694,#14695,#14696,
#14697));
#14786=CLOSED_SHELL('',(#14698,#14699,#14700,#14701,#14702,#14703));
#14787=CLOSED_SHELL('',(#14704,#14705,#14706,#14707,#14708,#14709,#14710,
#14711,#14712,#14713,#14714,#14715,#14716,#14717,#14718,#14719,#14720,#14721,
#14722));
#14788=CLOSED_SHELL('',(#14723,#14724,#14725,#14726,#14727,#14728,#14729,
#14730,#14731,#14732,#14733,#14734,#14735,#14736,#14737,#14738,#14739,#14740,
#14741,#14742,#14743,#14744,#14745,#14746,#14747,#14748,#14749,#14750,#14751,
#14752,#14753,#14754,#14755,#14756,#14757,#14758,#14759,#14760,#14761,#14762,
#14763,#14764,#14765,#14766,#14767,#14768,#14769,#14770,#14771,#14772,#14773,
#14774,#14775));
#14789=DERIVED_UNIT_ELEMENT(#14815,1.);
#14790=DERIVED_UNIT_ELEMENT(#37183,-3.);
#14791=DERIVED_UNIT_ELEMENT(#14815,1.);
#14792=DERIVED_UNIT_ELEMENT(#37183,-3.);
#14793=DERIVED_UNIT_ELEMENT(#14815,1.);
#14794=DERIVED_UNIT_ELEMENT(#37183,-3.);
#14795=DERIVED_UNIT_ELEMENT(#14815,1.);
#14796=DERIVED_UNIT_ELEMENT(#37183,-3.);
#14797=DERIVED_UNIT_ELEMENT(#14815,1.);
#14798=DERIVED_UNIT_ELEMENT(#37183,-3.);
#14799=DERIVED_UNIT_ELEMENT(#14815,1.);
#14800=DERIVED_UNIT_ELEMENT(#37183,-3.);
#14801=DERIVED_UNIT_ELEMENT(#14815,1.);
#14802=DERIVED_UNIT_ELEMENT(#37183,-3.);
#14803=DERIVED_UNIT_ELEMENT(#14815,1.);
#14804=DERIVED_UNIT_ELEMENT(#37183,-3.);
#14805=DERIVED_UNIT_ELEMENT(#14815,1.);
#14806=DERIVED_UNIT_ELEMENT(#37183,-3.);
#14807=DERIVED_UNIT_ELEMENT(#14815,1.);
#14808=DERIVED_UNIT_ELEMENT(#37183,-3.);
#14809=DERIVED_UNIT_ELEMENT(#14815,1.);
#14810=DERIVED_UNIT_ELEMENT(#37183,-3.);
#14811=DERIVED_UNIT_ELEMENT(#14815,1.);
#14812=DERIVED_UNIT_ELEMENT(#37183,-3.);
#14813=DERIVED_UNIT_ELEMENT(#14815,1.);
#14814=DERIVED_UNIT_ELEMENT(#37183,-3.);
#14815=(
MASS_UNIT()
NAMED_UNIT(*)
SI_UNIT(.KILO.,.GRAM.)
);
#14816=DERIVED_UNIT((#14789,#14790));
#14817=DERIVED_UNIT((#14791,#14792));
#14818=DERIVED_UNIT((#14793,#14794));
#14819=DERIVED_UNIT((#14795,#14796));
#14820=DERIVED_UNIT((#14797,#14798));
#14821=DERIVED_UNIT((#14799,#14800));
#14822=DERIVED_UNIT((#14801,#14802));
#14823=DERIVED_UNIT((#14803,#14804));
#14824=DERIVED_UNIT((#14805,#14806));
#14825=DERIVED_UNIT((#14807,#14808));
#14826=DERIVED_UNIT((#14809,#14810));
#14827=DERIVED_UNIT((#14811,#14812));
#14828=DERIVED_UNIT((#14813,#14814));
#14829=MEASURE_REPRESENTATION_ITEM('density measure',
POSITIVE_RATIO_MEASURE(7850.),#14816);
#14830=MEASURE_REPRESENTATION_ITEM('density measure',
POSITIVE_RATIO_MEASURE(7850.),#14817);
#14831=MEASURE_REPRESENTATION_ITEM('density measure',
POSITIVE_RATIO_MEASURE(7850.),#14818);
#14832=MEASURE_REPRESENTATION_ITEM('density measure',
POSITIVE_RATIO_MEASURE(7850.),#14819);
#14833=MEASURE_REPRESENTATION_ITEM('density measure',
POSITIVE_RATIO_MEASURE(7850.),#14820);
#14834=MEASURE_REPRESENTATION_ITEM('density measure',
POSITIVE_RATIO_MEASURE(7850.),#14821);
#14835=MEASURE_REPRESENTATION_ITEM('density measure',
POSITIVE_RATIO_MEASURE(7850.),#14822);
#14836=MEASURE_REPRESENTATION_ITEM('density measure',
POSITIVE_RATIO_MEASURE(7850.),#14823);
#14837=MEASURE_REPRESENTATION_ITEM('density measure',
POSITIVE_RATIO_MEASURE(7850.),#14824);
#14838=MEASURE_REPRESENTATION_ITEM('density measure',
POSITIVE_RATIO_MEASURE(7850.),#14825);
#14839=MEASURE_REPRESENTATION_ITEM('density measure',
POSITIVE_RATIO_MEASURE(7850.),#14826);
#14840=MEASURE_REPRESENTATION_ITEM('density measure',
POSITIVE_RATIO_MEASURE(7850.),#14827);
#14841=MEASURE_REPRESENTATION_ITEM('density measure',
POSITIVE_RATIO_MEASURE(7850.),#14828);
#14842=PROPERTY_DEFINITION_REPRESENTATION(#14907,#14868);
#14843=PROPERTY_DEFINITION_REPRESENTATION(#14908,#14869);
#14844=PROPERTY_DEFINITION_REPRESENTATION(#14909,#14870);
#14845=PROPERTY_DEFINITION_REPRESENTATION(#14910,#14871);
#14846=PROPERTY_DEFINITION_REPRESENTATION(#14911,#14872);
#14847=PROPERTY_DEFINITION_REPRESENTATION(#14912,#14873);
#14848=PROPERTY_DEFINITION_REPRESENTATION(#14913,#14874);
#14849=PROPERTY_DEFINITION_REPRESENTATION(#14914,#14875);
#14850=PROPERTY_DEFINITION_REPRESENTATION(#14915,#14876);
#14851=PROPERTY_DEFINITION_REPRESENTATION(#14916,#14877);
#14852=PROPERTY_DEFINITION_REPRESENTATION(#14917,#14878);
#14853=PROPERTY_DEFINITION_REPRESENTATION(#14918,#14879);
#14854=PROPERTY_DEFINITION_REPRESENTATION(#14919,#14880);
#14855=PROPERTY_DEFINITION_REPRESENTATION(#14920,#14881);
#14856=PROPERTY_DEFINITION_REPRESENTATION(#14921,#14882);
#14857=PROPERTY_DEFINITION_REPRESENTATION(#14922,#14883);
#14858=PROPERTY_DEFINITION_REPRESENTATION(#14923,#14884);
#14859=PROPERTY_DEFINITION_REPRESENTATION(#14924,#14885);
#14860=PROPERTY_DEFINITION_REPRESENTATION(#14925,#14886);
#14861=PROPERTY_DEFINITION_REPRESENTATION(#14926,#14887);
#14862=PROPERTY_DEFINITION_REPRESENTATION(#14927,#14888);
#14863=PROPERTY_DEFINITION_REPRESENTATION(#14928,#14889);
#14864=PROPERTY_DEFINITION_REPRESENTATION(#14929,#14890);
#14865=PROPERTY_DEFINITION_REPRESENTATION(#14930,#14891);
#14866=PROPERTY_DEFINITION_REPRESENTATION(#14931,#14892);
#14867=PROPERTY_DEFINITION_REPRESENTATION(#14932,#14893);
#14868=REPRESENTATION('material name',(#14894),#37168);
#14869=REPRESENTATION('density',(#14829),#37168);
#14870=REPRESENTATION('material name',(#14895),#37169);
#14871=REPRESENTATION('density',(#14830),#37169);
#14872=REPRESENTATION('material name',(#14896),#37170);
#14873=REPRESENTATION('density',(#14831),#37170);
#14874=REPRESENTATION('material name',(#14897),#37171);
#14875=REPRESENTATION('density',(#14832),#37171);
#14876=REPRESENTATION('material name',(#14898),#37172);
#14877=REPRESENTATION('density',(#14833),#37172);
#14878=REPRESENTATION('material name',(#14899),#37173);
#14879=REPRESENTATION('density',(#14834),#37173);
#14880=REPRESENTATION('material name',(#14900),#37174);
#14881=REPRESENTATION('density',(#14835),#37174);
#14882=REPRESENTATION('material name',(#14901),#37175);
#14883=REPRESENTATION('density',(#14836),#37175);
#14884=REPRESENTATION('material name',(#14902),#37176);
#14885=REPRESENTATION('density',(#14837),#37176);
#14886=REPRESENTATION('material name',(#14903),#37177);
#14887=REPRESENTATION('density',(#14838),#37177);
#14888=REPRESENTATION('material name',(#14904),#37178);
#14889=REPRESENTATION('density',(#14839),#37178);
#14890=REPRESENTATION('material name',(#14905),#37179);
#14891=REPRESENTATION('density',(#14840),#37179);
#14892=REPRESENTATION('material name',(#14906),#37180);
#14893=REPRESENTATION('density',(#14841),#37180);
#14894=DESCRIPTIVE_REPRESENTATION_ITEM('Steel','Steel');
#14895=DESCRIPTIVE_REPRESENTATION_ITEM('Steel','Steel');
#14896=DESCRIPTIVE_REPRESENTATION_ITEM('Steel','Steel');
#14897=DESCRIPTIVE_REPRESENTATION_ITEM('Steel','Steel');
#14898=DESCRIPTIVE_REPRESENTATION_ITEM('Steel','Steel');
#14899=DESCRIPTIVE_REPRESENTATION_ITEM('Steel','Steel');
#14900=DESCRIPTIVE_REPRESENTATION_ITEM('Steel','Steel');
#14901=DESCRIPTIVE_REPRESENTATION_ITEM('Steel','Steel');
#14902=DESCRIPTIVE_REPRESENTATION_ITEM('Steel','Steel');
#14903=DESCRIPTIVE_REPRESENTATION_ITEM('Steel','Steel');
#14904=DESCRIPTIVE_REPRESENTATION_ITEM('Steel','Steel');
#14905=DESCRIPTIVE_REPRESENTATION_ITEM('Steel','Steel');
#14906=DESCRIPTIVE_REPRESENTATION_ITEM('Steel','Steel');
#14907=PROPERTY_DEFINITION('material property','material name',#37253);
#14908=PROPERTY_DEFINITION('material property','density of part',#37253);
#14909=PROPERTY_DEFINITION('material property','material name',#37254);
#14910=PROPERTY_DEFINITION('material property','density of part',#37254);
#14911=PROPERTY_DEFINITION('material property','material name',#37255);
#14912=PROPERTY_DEFINITION('material property','density of part',#37255);
#14913=PROPERTY_DEFINITION('material property','material name',#37256);
#14914=PROPERTY_DEFINITION('material property','density of part',#37256);
#14915=PROPERTY_DEFINITION('material property','material name',#37257);
#14916=PROPERTY_DEFINITION('material property','density of part',#37257);
#14917=PROPERTY_DEFINITION('material property','material name',#37258);
#14918=PROPERTY_DEFINITION('material property','density of part',#37258);
#14919=PROPERTY_DEFINITION('material property','material name',#37259);
#14920=PROPERTY_DEFINITION('material property','density of part',#37259);
#14921=PROPERTY_DEFINITION('material property','material name',#37260);
#14922=PROPERTY_DEFINITION('material property','density of part',#37260);
#14923=PROPERTY_DEFINITION('material property','material name',#37261);
#14924=PROPERTY_DEFINITION('material property','density of part',#37261);
#14925=PROPERTY_DEFINITION('material property','material name',#37262);
#14926=PROPERTY_DEFINITION('material property','density of part',#37262);
#14927=PROPERTY_DEFINITION('material property','material name',#37263);
#14928=PROPERTY_DEFINITION('material property','density of part',#37263);
#14929=PROPERTY_DEFINITION('material property','material name',#37264);
#14930=PROPERTY_DEFINITION('material property','density of part',#37264);
#14931=PROPERTY_DEFINITION('material property','material name',#37265);
#14932=PROPERTY_DEFINITION('material property','density of part',#37265);
#14933=AXIS2_PLACEMENT_3D('',#19748,#16125,#16126);
#14934=AXIS2_PLACEMENT_3D('',#19749,#16127,#16128);
#14935=AXIS2_PLACEMENT_3D('',#19750,#16129,#16130);
#14936=AXIS2_PLACEMENT_3D('',#19767,#16135,#16136);
#14937=AXIS2_PLACEMENT_3D('',#19777,#16140,#16141);
#14938=AXIS2_PLACEMENT_3D('',#19779,#16142,#16143);
#14939=AXIS2_PLACEMENT_3D('',#19788,#16144,#16145);
#14940=AXIS2_PLACEMENT_3D('',#19789,#16146,#16147);
#14941=AXIS2_PLACEMENT_3D('',#19791,#16148,#16149);
#14942=AXIS2_PLACEMENT_3D('',#19793,#16151,#16152);
#14943=AXIS2_PLACEMENT_3D('',#19797,#16155,#16156);
#14944=AXIS2_PLACEMENT_3D('',#19804,#16160,#16161);
#14945=AXIS2_PLACEMENT_3D('',#19810,#16165,#16166);
#14946=AXIS2_PLACEMENT_3D('',#19812,#16167,#16168);
#14947=AXIS2_PLACEMENT_3D('',#19815,#16170,#16171);
#14948=AXIS2_PLACEMENT_3D('',#19816,#16172,#16173);
#14949=AXIS2_PLACEMENT_3D('',#19824,#16176,#16177);
#14950=AXIS2_PLACEMENT_3D('',#19831,#16180,#16181);
#14951=AXIS2_PLACEMENT_3D('',#19834,#16184,#16185);
#14952=AXIS2_PLACEMENT_3D('',#19845,#16189,#16190);
#14953=AXIS2_PLACEMENT_3D('',#19847,#16191,#16192);
#14954=AXIS2_PLACEMENT_3D('',#19850,#16194,#16195);
#14955=AXIS2_PLACEMENT_3D('',#19851,#16196,#16197);
#14956=AXIS2_PLACEMENT_3D('',#19854,#16200,#16201);
#14957=AXIS2_PLACEMENT_3D('',#19856,#16202,#16203);
#14958=AXIS2_PLACEMENT_3D('',#19860,#16205,#16206);
#14959=AXIS2_PLACEMENT_3D('',#19865,#16209,#16210);
#14960=AXIS2_PLACEMENT_3D('',#19866,#16211,#16212);
#14961=AXIS2_PLACEMENT_3D('',#19868,#16214,#16215);
#14962=AXIS2_PLACEMENT_3D('',#19870,#16217,#16218);
#14963=AXIS2_PLACEMENT_3D('',#19881,#16220,#16221);
#14964=AXIS2_PLACEMENT_3D('',#19882,#16222,#16223);
#14965=AXIS2_PLACEMENT_3D('',#19892,#16227,#16228);
#14966=AXIS2_PLACEMENT_3D('',#19898,#16232,#16233);
#14967=AXIS2_PLACEMENT_3D('',#19902,#16236,#16237);
#14968=AXIS2_PLACEMENT_3D('',#19908,#16241,#16242);
#14969=AXIS2_PLACEMENT_3D('',#19913,#16244,#16245);
#14970=AXIS2_PLACEMENT_3D('',#19921,#16248,#16249);
#14971=AXIS2_PLACEMENT_3D('',#19923,#16250,#16251);
#14972=AXIS2_PLACEMENT_3D('',#19925,#16253,#16254);
#14973=AXIS2_PLACEMENT_3D('',#19927,#16256,#16257);
#14974=AXIS2_PLACEMENT_3D('',#19930,#16260,#16261);
#14975=AXIS2_PLACEMENT_3D('',#19936,#16265,#16266);
#14976=AXIS2_PLACEMENT_3D('',#19938,#16267,#16268);
#14977=AXIS2_PLACEMENT_3D('',#19941,#16270,#16271);
#14978=AXIS2_PLACEMENT_3D('',#19942,#16272,#16273);
#14979=AXIS2_PLACEMENT_3D('',#19950,#16276,#16277);
#14980=AXIS2_PLACEMENT_3D('',#19951,#16278,#16279);
#14981=AXIS2_PLACEMENT_3D('',#19953,#16280,#16281);
#14982=AXIS2_PLACEMENT_3D('',#19954,#16282,#16283);
#14983=AXIS2_PLACEMENT_3D('',#19959,#16284,#16285);
#14984=AXIS2_PLACEMENT_3D('',#19960,#16286,#16287);
#14985=AXIS2_PLACEMENT_3D('',#19965,#16288,#16289);
#14986=AXIS2_PLACEMENT_3D('',#19966,#16290,#16291);
#14987=AXIS2_PLACEMENT_3D('',#19967,#16292,#16293);
#14988=AXIS2_PLACEMENT_3D('',#19969,#16295,#16296);
#14989=AXIS2_PLACEMENT_3D('',#19972,#16298,#16299);
#14990=AXIS2_PLACEMENT_3D('',#19973,#16300,#16301);
#14991=AXIS2_PLACEMENT_3D('',#19975,#16302,#16303);
#14992=AXIS2_PLACEMENT_3D('',#19977,#16305,#16306);
#14993=AXIS2_PLACEMENT_3D('',#19978,#16307,#16308);
#14994=AXIS2_PLACEMENT_3D('',#19981,#16311,#16312);
#14995=AXIS2_PLACEMENT_3D('',#19982,#16313,#16314);
#14996=AXIS2_PLACEMENT_3D('',#19983,#16315,#16316);
#14997=AXIS2_PLACEMENT_3D('',#19984,#16317,#16318);
#14998=AXIS2_PLACEMENT_3D('',#19985,#16319,#16320);
#14999=AXIS2_PLACEMENT_3D('',#19994,#16325,#16326);
#15000=AXIS2_PLACEMENT_3D('',#19996,#16327,#16328);
#15001=AXIS2_PLACEMENT_3D('',#19999,#16330,#16331);
#15002=AXIS2_PLACEMENT_3D('',#20000,#16332,#16333);
#15003=AXIS2_PLACEMENT_3D('',#20006,#16337,#16338);
#15004=AXIS2_PLACEMENT_3D('',#20008,#16339,#16340);
#15005=AXIS2_PLACEMENT_3D('',#20011,#16342,#16343);
#15006=AXIS2_PLACEMENT_3D('',#20012,#16344,#16345);
#15007=AXIS2_PLACEMENT_3D('',#20018,#16349,#16350);
#15008=AXIS2_PLACEMENT_3D('',#20026,#16353,#16354);
#15009=AXIS2_PLACEMENT_3D('',#20029,#16356,#16357);
#15010=AXIS2_PLACEMENT_3D('',#20030,#16358,#16359);
#15011=AXIS2_PLACEMENT_3D('',#20042,#16362,#16363);
#15012=AXIS2_PLACEMENT_3D('',#20051,#16368,#16369);
#15013=AXIS2_PLACEMENT_3D('',#20060,#16374,#16375);
#15014=AXIS2_PLACEMENT_3D('',#20066,#16379,#16380);
#15015=AXIS2_PLACEMENT_3D('',#20070,#16382,#16383);
#15016=AXIS2_PLACEMENT_3D('',#20071,#16384,#16385);
#15017=AXIS2_PLACEMENT_3D('',#20072,#16386,#16387);
#15018=AXIS2_PLACEMENT_3D('',#20080,#16392,#16393);
#15019=AXIS2_PLACEMENT_3D('',#20084,#16395,#16396);
#15020=AXIS2_PLACEMENT_3D('',#20085,#16397,#16398);
#15021=AXIS2_PLACEMENT_3D('',#20086,#16399,#16400);
#15022=AXIS2_PLACEMENT_3D('',#20092,#16404,#16405);
#15023=AXIS2_PLACEMENT_3D('',#20096,#16407,#16408);
#15024=AXIS2_PLACEMENT_3D('',#20097,#16409,#16410);
#15025=AXIS2_PLACEMENT_3D('',#20098,#16411,#16412);
#15026=AXIS2_PLACEMENT_3D('',#20101,#16415,#16416);
#15027=AXIS2_PLACEMENT_3D('',#20103,#16417,#16418);
#15028=AXIS2_PLACEMENT_3D('',#20106,#16420,#16421);
#15029=AXIS2_PLACEMENT_3D('',#20107,#16422,#16423);
#15030=AXIS2_PLACEMENT_3D('',#20115,#16428,#16429);
#15031=AXIS2_PLACEMENT_3D('',#20119,#16431,#16432);
#15032=AXIS2_PLACEMENT_3D('',#20131,#16438,#16439);
#15033=AXIS2_PLACEMENT_3D('',#20137,#16442,#16443);
#15034=AXIS2_PLACEMENT_3D('',#20140,#16446,#16447);
#15035=AXIS2_PLACEMENT_3D('',#20142,#16449,#16450);
#15036=AXIS2_PLACEMENT_3D('',#20144,#16452,#16453);
#15037=AXIS2_PLACEMENT_3D('',#20146,#16455,#16456);
#15038=AXIS2_PLACEMENT_3D('',#20150,#16458,#16459);
#15039=AXIS2_PLACEMENT_3D('',#20156,#16462,#16463);
#15040=AXIS2_PLACEMENT_3D('',#20167,#16469,#16470);
#15041=AXIS2_PLACEMENT_3D('',#20168,#16471,#16472);
#15042=AXIS2_PLACEMENT_3D('',#20178,#16476,#16477);
#15043=AXIS2_PLACEMENT_3D('',#20186,#16480,#16481);
#15044=AXIS2_PLACEMENT_3D('',#20200,#16485,#16486);
#15045=AXIS2_PLACEMENT_3D('',#20206,#16490,#16491);
#15046=AXIS2_PLACEMENT_3D('',#20214,#16496,#16497);
#15047=AXIS2_PLACEMENT_3D('',#20218,#16500,#16501);
#15048=AXIS2_PLACEMENT_3D('',#20220,#16502,#16503);
#15049=AXIS2_PLACEMENT_3D('',#20222,#16505,#16506);
#15050=AXIS2_PLACEMENT_3D('',#20226,#16509,#16510);
#15051=AXIS2_PLACEMENT_3D('',#20234,#16513,#16514);
#15052=AXIS2_PLACEMENT_3D('',#20238,#16516,#16517);
#15053=AXIS2_PLACEMENT_3D('',#20240,#16519,#16520);
#15054=AXIS2_PLACEMENT_3D('',#20242,#16522,#16523);
#15055=AXIS2_PLACEMENT_3D('',#20245,#16526,#16527);
#15056=AXIS2_PLACEMENT_3D('',#20253,#16530,#16531);
#15057=AXIS2_PLACEMENT_3D('',#20256,#16533,#16534);
#15058=AXIS2_PLACEMENT_3D('',#20257,#16535,#16536);
#15059=AXIS2_PLACEMENT_3D('',#20267,#16538,#16539);
#15060=AXIS2_PLACEMENT_3D('',#20269,#16541,#16542);
#15061=AXIS2_PLACEMENT_3D('',#20273,#16545,#16546);
#15062=AXIS2_PLACEMENT_3D('',#20277,#16549,#16550);
#15063=AXIS2_PLACEMENT_3D('',#20281,#16552,#16553);
#15064=AXIS2_PLACEMENT_3D('',#20282,#16554,#16555);
#15065=AXIS2_PLACEMENT_3D('',#20283,#16556,#16557);
#15066=AXIS2_PLACEMENT_3D('',#20289,#16561,#16562);
#15067=AXIS2_PLACEMENT_3D('',#20292,#16564,#16565);
#15068=AXIS2_PLACEMENT_3D('',#20293,#16566,#16567);
#15069=AXIS2_PLACEMENT_3D('',#20294,#16568,#16569);
#15070=AXIS2_PLACEMENT_3D('',#20296,#16571,#16572);
#15071=AXIS2_PLACEMENT_3D('',#20299,#16574,#16575);
#15072=AXIS2_PLACEMENT_3D('',#20300,#16576,#16577);
#15073=AXIS2_PLACEMENT_3D('',#20302,#16578,#16579);
#15074=AXIS2_PLACEMENT_3D('',#20303,#16580,#16581);
#15075=AXIS2_PLACEMENT_3D('',#20308,#16585,#16586);
#15076=AXIS2_PLACEMENT_3D('',#20312,#16587,#16588);
#15077=AXIS2_PLACEMENT_3D('',#20316,#16590,#16591);
#15078=AXIS2_PLACEMENT_3D('',#20317,#16592,#16593);
#15079=AXIS2_PLACEMENT_3D('',#20318,#16594,#16595);
#15080=AXIS2_PLACEMENT_3D('',#20324,#16599,#16600);
#15081=AXIS2_PLACEMENT_3D('',#20327,#16602,#16603);
#15082=AXIS2_PLACEMENT_3D('',#20328,#16604,#16605);
#15083=AXIS2_PLACEMENT_3D('',#20329,#16606,#16607);
#15084=AXIS2_PLACEMENT_3D('',#20331,#16609,#16610);
#15085=AXIS2_PLACEMENT_3D('',#20333,#16611,#16612);
#15086=AXIS2_PLACEMENT_3D('',#20334,#16613,#16614);
#15087=AXIS2_PLACEMENT_3D('',#20338,#16615,#16616);
#15088=AXIS2_PLACEMENT_3D('',#20348,#16620,#16621);
#15089=AXIS2_PLACEMENT_3D('',#20351,#16624,#16625);
#15090=AXIS2_PLACEMENT_3D('',#20353,#16626,#16627);
#15091=AXIS2_PLACEMENT_3D('',#20357,#16628,#16629);
#15092=AXIS2_PLACEMENT_3D('',#20359,#16631,#16632);
#15093=AXIS2_PLACEMENT_3D('',#20364,#16633,#16634);
#15094=AXIS2_PLACEMENT_3D('',#20365,#16635,#16636);
#15095=AXIS2_PLACEMENT_3D('',#20371,#16639,#16640);
#15096=AXIS2_PLACEMENT_3D('',#20374,#16642,#16643);
#15097=AXIS2_PLACEMENT_3D('',#20375,#16644,#16645);
#15098=AXIS2_PLACEMENT_3D('',#20377,#16647,#16648);
#15099=AXIS2_PLACEMENT_3D('',#20389,#16650,#16651);
#15100=AXIS2_PLACEMENT_3D('',#20401,#16653,#16654);
#15101=AXIS2_PLACEMENT_3D('',#20404,#16655,#16656);
#15102=AXIS2_PLACEMENT_3D('',#20411,#16657,#16658);
#15103=AXIS2_PLACEMENT_3D('',#20417,#16659,#16660);
#15104=AXIS2_PLACEMENT_3D('',#20421,#16661,#16662);
#15105=AXIS2_PLACEMENT_3D('',#20427,#16665,#16666);
#15106=AXIS2_PLACEMENT_3D('',#20431,#16669,#16670);
#15107=AXIS2_PLACEMENT_3D('',#20435,#16673,#16674);
#15108=AXIS2_PLACEMENT_3D('',#20450,#16677,#16678);
#15109=AXIS2_PLACEMENT_3D('',#20465,#16681,#16682);
#15110=AXIS2_PLACEMENT_3D('',#20469,#16683,#16684);
#15111=AXIS2_PLACEMENT_3D('',#20473,#16685,#16686);
#15112=AXIS2_PLACEMENT_3D('',#20474,#16687,#16688);
#15113=AXIS2_PLACEMENT_3D('',#20480,#16689,#16690);
#15114=AXIS2_PLACEMENT_3D('',#20484,#16691,#16692);
#15115=AXIS2_PLACEMENT_3D('',#20489,#16696,#16697);
#15116=AXIS2_PLACEMENT_3D('',#20490,#16698,#16699);
#15117=AXIS2_PLACEMENT_3D('',#20491,#16700,#16701);
#15118=AXIS2_PLACEMENT_3D('',#20492,#16702,#16703);
#15119=AXIS2_PLACEMENT_3D('',#20493,#16704,#16705);
#15120=AXIS2_PLACEMENT_3D('',#20494,#16706,#16707);
#15121=AXIS2_PLACEMENT_3D('',#20496,#16708,#16709);
#15122=AXIS2_PLACEMENT_3D('',#20497,#16710,#16711);
#15123=AXIS2_PLACEMENT_3D('',#20498,#16712,#16713);
#15124=AXIS2_PLACEMENT_3D('',#20500,#16715,#16716);
#15125=AXIS2_PLACEMENT_3D('',#20501,#16717,#16718);
#15126=AXIS2_PLACEMENT_3D('',#20503,#16720,#16721);
#15127=AXIS2_PLACEMENT_3D('',#20506,#16723,#16724);
#15128=AXIS2_PLACEMENT_3D('',#20507,#16725,#16726);
#15129=AXIS2_PLACEMENT_3D('',#20509,#16727,#16728);
#15130=AXIS2_PLACEMENT_3D('',#20511,#16730,#16731);
#15131=AXIS2_PLACEMENT_3D('',#20513,#16733,#16734);
#15132=AXIS2_PLACEMENT_3D('',#20515,#16736,#16737);
#15133=AXIS2_PLACEMENT_3D('',#20517,#16739,#16740);
#15134=AXIS2_PLACEMENT_3D('',#20519,#16742,#16743);
#15135=AXIS2_PLACEMENT_3D('',#20521,#16745,#16746);
#15136=AXIS2_PLACEMENT_3D('',#20522,#16747,#16748);
#15137=AXIS2_PLACEMENT_3D('',#20523,#16749,#16750);
#15138=AXIS2_PLACEMENT_3D('',#20524,#16751,#16752);
#15139=AXIS2_PLACEMENT_3D('',#20533,#16757,#16758);
#15140=AXIS2_PLACEMENT_3D('',#20537,#16760,#16761);
#15141=AXIS2_PLACEMENT_3D('',#20538,#16762,#16763);
#15142=AXIS2_PLACEMENT_3D('',#20539,#16764,#16765);
#15143=AXIS2_PLACEMENT_3D('',#20545,#16769,#16770);
#15144=AXIS2_PLACEMENT_3D('',#20551,#16774,#16775);
#15145=AXIS2_PLACEMENT_3D('',#20554,#16777,#16778);
#15146=AXIS2_PLACEMENT_3D('',#20555,#16779,#16780);
#15147=AXIS2_PLACEMENT_3D('',#20559,#16783,#16784);
#15148=AXIS2_PLACEMENT_3D('',#20565,#16788,#16789);
#15149=AXIS2_PLACEMENT_3D('',#20568,#16791,#16792);
#15150=AXIS2_PLACEMENT_3D('',#20569,#16793,#16794);
#15151=AXIS2_PLACEMENT_3D('',#20573,#16797,#16798);
#15152=AXIS2_PLACEMENT_3D('',#20587,#16806,#16807);
#15153=AXIS2_PLACEMENT_3D('',#20596,#16812,#16813);
#15154=AXIS2_PLACEMENT_3D('',#20600,#16815,#16816);
#15155=AXIS2_PLACEMENT_3D('',#20601,#16817,#16818);
#15156=AXIS2_PLACEMENT_3D('',#20602,#16819,#16820);
#15157=AXIS2_PLACEMENT_3D('',#20608,#16824,#16825);
#15158=AXIS2_PLACEMENT_3D('',#20614,#16829,#16830);
#15159=AXIS2_PLACEMENT_3D('',#20617,#16832,#16833);
#15160=AXIS2_PLACEMENT_3D('',#20618,#16834,#16835);
#15161=AXIS2_PLACEMENT_3D('',#20622,#16838,#16839);
#15162=AXIS2_PLACEMENT_3D('',#20629,#16843,#16844);
#15163=AXIS2_PLACEMENT_3D('',#20635,#16848,#16849);
#15164=AXIS2_PLACEMENT_3D('',#20643,#16854,#16855);
#15165=AXIS2_PLACEMENT_3D('',#20651,#16860,#16861);
#15166=AXIS2_PLACEMENT_3D('',#20655,#16864,#16865);
#15167=AXIS2_PLACEMENT_3D('',#20659,#16868,#16869);
#15168=AXIS2_PLACEMENT_3D('',#20665,#16873,#16874);
#15169=AXIS2_PLACEMENT_3D('',#20667,#16875,#16876);
#15170=AXIS2_PLACEMENT_3D('',#20670,#16878,#16879);
#15171=AXIS2_PLACEMENT_3D('',#20671,#16880,#16881);
#15172=AXIS2_PLACEMENT_3D('',#20674,#16883,#16884);
#15173=AXIS2_PLACEMENT_3D('',#20675,#16885,#16886);
#15174=AXIS2_PLACEMENT_3D('',#20677,#16888,#16889);
#15175=AXIS2_PLACEMENT_3D('',#20679,#16890,#16891);
#15176=AXIS2_PLACEMENT_3D('',#20682,#16893,#16894);
#15177=AXIS2_PLACEMENT_3D('',#20683,#16895,#16896);
#15178=AXIS2_PLACEMENT_3D('',#20686,#16898,#16899);
#15179=AXIS2_PLACEMENT_3D('',#20687,#16900,#16901);
#15180=AXIS2_PLACEMENT_3D('',#20689,#16903,#16904);
#15181=AXIS2_PLACEMENT_3D('',#20692,#16906,#16907);
#15182=AXIS2_PLACEMENT_3D('',#20693,#16908,#16909);
#15183=AXIS2_PLACEMENT_3D('',#20706,#16916,#16917);
#15184=AXIS2_PLACEMENT_3D('',#20712,#16921,#16922);
#15185=AXIS2_PLACEMENT_3D('',#20716,#16925,#16926);
#15186=AXIS2_PLACEMENT_3D('',#20722,#16930,#16931);
#15187=AXIS2_PLACEMENT_3D('',#20726,#16934,#16935);
#15188=AXIS2_PLACEMENT_3D('',#20728,#16937,#16938);
#15189=AXIS2_PLACEMENT_3D('',#20730,#16940,#16941);
#15190=AXIS2_PLACEMENT_3D('',#20733,#16944,#16945);
#15191=AXIS2_PLACEMENT_3D('',#20735,#16947,#16948);
#15192=AXIS2_PLACEMENT_3D('',#20737,#16950,#16951);
#15193=AXIS2_PLACEMENT_3D('',#20740,#16953,#16954);
#15194=AXIS2_PLACEMENT_3D('',#20741,#16955,#16956);
#15195=AXIS2_PLACEMENT_3D('',#20754,#16963,#16964);
#15196=AXIS2_PLACEMENT_3D('',#20760,#16968,#16969);
#15197=AXIS2_PLACEMENT_3D('',#20763,#16971,#16972);
#15198=AXIS2_PLACEMENT_3D('',#20764,#16973,#16974);
#15199=AXIS2_PLACEMENT_3D('',#20768,#16977,#16978);
#15200=AXIS2_PLACEMENT_3D('',#20777,#16983,#16984);
#15201=AXIS2_PLACEMENT_3D('',#20783,#16988,#16989);
#15202=AXIS2_PLACEMENT_3D('',#20792,#16994,#16995);
#15203=AXIS2_PLACEMENT_3D('',#20798,#16999,#17000);
#15204=AXIS2_PLACEMENT_3D('',#20801,#17003,#17004);
#15205=AXIS2_PLACEMENT_3D('',#20804,#17007,#17008);
#15206=AXIS2_PLACEMENT_3D('',#20807,#17011,#17012);
#15207=AXIS2_PLACEMENT_3D('',#20809,#17014,#17015);
#15208=AXIS2_PLACEMENT_3D('',#20811,#17017,#17018);
#15209=AXIS2_PLACEMENT_3D('',#20813,#17020,#17021);
#15210=AXIS2_PLACEMENT_3D('',#20820,#17025,#17026);
#15211=AXIS2_PLACEMENT_3D('',#20826,#17030,#17031);
#15212=AXIS2_PLACEMENT_3D('',#20833,#17035,#17036);
#15213=AXIS2_PLACEMENT_3D('',#20839,#17040,#17041);
#15214=AXIS2_PLACEMENT_3D('',#20847,#17046,#17047);
#15215=AXIS2_PLACEMENT_3D('',#20850,#17050,#17051);
#15216=AXIS2_PLACEMENT_3D('',#20858,#17056,#17057);
#15217=AXIS2_PLACEMENT_3D('',#20860,#17059,#17060);
#15218=AXIS2_PLACEMENT_3D('',#20864,#17063,#17064);
#15219=AXIS2_PLACEMENT_3D('',#20870,#17068,#17069);
#15220=AXIS2_PLACEMENT_3D('',#20877,#17073,#17074);
#15221=AXIS2_PLACEMENT_3D('',#20883,#17078,#17079);
#15222=AXIS2_PLACEMENT_3D('',#20890,#17083,#17084);
#15223=AXIS2_PLACEMENT_3D('',#20896,#17088,#17089);
#15224=AXIS2_PLACEMENT_3D('',#20904,#17094,#17095);
#15225=AXIS2_PLACEMENT_3D('',#20907,#17098,#17099);
#15226=AXIS2_PLACEMENT_3D('',#20915,#17104,#17105);
#15227=AXIS2_PLACEMENT_3D('',#20917,#17107,#17108);
#15228=AXIS2_PLACEMENT_3D('',#20921,#17111,#17112);
#15229=AXIS2_PLACEMENT_3D('',#20927,#17116,#17117);
#15230=AXIS2_PLACEMENT_3D('',#20935,#17122,#17123);
#15231=AXIS2_PLACEMENT_3D('',#20939,#17126,#17127);
#15232=AXIS2_PLACEMENT_3D('',#20945,#17131,#17132);
#15233=AXIS2_PLACEMENT_3D('',#20954,#17137,#17138);
#15234=AXIS2_PLACEMENT_3D('',#20960,#17142,#17143);
#15235=AXIS2_PLACEMENT_3D('',#20966,#17147,#17148);
#15236=AXIS2_PLACEMENT_3D('',#20970,#17151,#17152);
#15237=AXIS2_PLACEMENT_3D('',#20976,#17156,#17157);
#15238=AXIS2_PLACEMENT_3D('',#20979,#17160,#17161);
#15239=AXIS2_PLACEMENT_3D('',#20986,#17164,#17165);
#15240=AXIS2_PLACEMENT_3D('',#21009,#17178,#17179);
#15241=AXIS2_PLACEMENT_3D('',#21011,#17181,#17182);
#15242=AXIS2_PLACEMENT_3D('',#21017,#17186,#17187);
#15243=AXIS2_PLACEMENT_3D('',#21021,#17189,#17190);
#15244=AXIS2_PLACEMENT_3D('',#21022,#17191,#17192);
#15245=AXIS2_PLACEMENT_3D('',#21023,#17193,#17194);
#15246=AXIS2_PLACEMENT_3D('',#21029,#17198,#17199);
#15247=AXIS2_PLACEMENT_3D('',#21033,#17201,#17202);
#15248=AXIS2_PLACEMENT_3D('',#21034,#17203,#17204);
#15249=AXIS2_PLACEMENT_3D('',#21035,#17205,#17206);
#15250=AXIS2_PLACEMENT_3D('',#21041,#17210,#17211);
#15251=AXIS2_PLACEMENT_3D('',#21045,#17213,#17214);
#15252=AXIS2_PLACEMENT_3D('',#21046,#17215,#17216);
#15253=AXIS2_PLACEMENT_3D('',#21047,#17217,#17218);
#15254=AXIS2_PLACEMENT_3D('',#21053,#17222,#17223);
#15255=AXIS2_PLACEMENT_3D('',#21054,#17224,#17225);
#15256=AXIS2_PLACEMENT_3D('',#21055,#17226,#17227);
#15257=AXIS2_PLACEMENT_3D('',#21056,#17228,#17229);
#15258=AXIS2_PLACEMENT_3D('',#21060,#17231,#17232);
#15259=AXIS2_PLACEMENT_3D('',#21062,#17234,#17235);
#15260=AXIS2_PLACEMENT_3D('',#21067,#17238,#17239);
#15261=AXIS2_PLACEMENT_3D('',#21068,#17240,#17241);
#15262=AXIS2_PLACEMENT_3D('',#21085,#17242,#17243);
#15263=AXIS2_PLACEMENT_3D('',#21086,#17244,#17245);
#15264=AXIS2_PLACEMENT_3D('',#21087,#17246,#17247);
#15265=AXIS2_PLACEMENT_3D('',#21091,#17250,#17251);
#15266=AXIS2_PLACEMENT_3D('',#21095,#17254,#17255);
#15267=AXIS2_PLACEMENT_3D('',#21098,#17258,#17259);
#15268=AXIS2_PLACEMENT_3D('',#21102,#17262,#17263);
#15269=AXIS2_PLACEMENT_3D('',#21104,#17264,#17265);
#15270=AXIS2_PLACEMENT_3D('',#21107,#17267,#17268);
#15271=AXIS2_PLACEMENT_3D('',#21108,#17269,#17270);
#15272=AXIS2_PLACEMENT_3D('',#21114,#17274,#17275);
#15273=AXIS2_PLACEMENT_3D('',#21116,#17276,#17277);
#15274=AXIS2_PLACEMENT_3D('',#21119,#17279,#17280);
#15275=AXIS2_PLACEMENT_3D('',#21120,#17281,#17282);
#15276=AXIS2_PLACEMENT_3D('',#21125,#17286,#17287);
#15277=AXIS2_PLACEMENT_3D('',#21128,#17289,#17290);
#15278=AXIS2_PLACEMENT_3D('',#21129,#17291,#17292);
#15279=AXIS2_PLACEMENT_3D('',#21133,#17295,#17296);
#15280=AXIS2_PLACEMENT_3D('',#21136,#17298,#17299);
#15281=AXIS2_PLACEMENT_3D('',#21137,#17300,#17301);
#15282=AXIS2_PLACEMENT_3D('',#21140,#17304,#17305);
#15283=AXIS2_PLACEMENT_3D('',#21142,#17307,#17308);
#15284=AXIS2_PLACEMENT_3D('',#21144,#17310,#17311);
#15285=AXIS2_PLACEMENT_3D('',#21146,#17313,#17314);
#15286=AXIS2_PLACEMENT_3D('',#21149,#17317,#17318);
#15287=AXIS2_PLACEMENT_3D('',#21151,#17320,#17321);
#15288=AXIS2_PLACEMENT_3D('',#21153,#17323,#17324);
#15289=AXIS2_PLACEMENT_3D('',#21155,#17326,#17327);
#15290=AXIS2_PLACEMENT_3D('',#21157,#17329,#17330);
#15291=AXIS2_PLACEMENT_3D('',#21174,#17331,#17332);
#15292=AXIS2_PLACEMENT_3D('',#21176,#17334,#17335);
#15293=AXIS2_PLACEMENT_3D('',#21177,#17336,#17337);
#15294=AXIS2_PLACEMENT_3D('',#21179,#17339,#17340);
#15295=AXIS2_PLACEMENT_3D('',#21180,#17341,#17342);
#15296=AXIS2_PLACEMENT_3D('',#21215,#17345,#17346);
#15297=AXIS2_PLACEMENT_3D('',#21219,#17348,#17349);
#15298=AXIS2_PLACEMENT_3D('',#21221,#17350,#17351);
#15299=AXIS2_PLACEMENT_3D('',#21263,#17353,#17354);
#15300=AXIS2_PLACEMENT_3D('',#21266,#17356,#17357);
#15301=AXIS2_PLACEMENT_3D('',#21304,#17360,#17361);
#15302=AXIS2_PLACEMENT_3D('',#21308,#17363,#17364);
#15303=AXIS2_PLACEMENT_3D('',#21350,#17366,#17367);
#15304=AXIS2_PLACEMENT_3D('',#21353,#17369,#17370);
#15305=AXIS2_PLACEMENT_3D('',#21354,#17371,#17372);
#15306=AXIS2_PLACEMENT_3D('',#21357,#17374,#17375);
#15307=AXIS2_PLACEMENT_3D('',#21358,#17376,#17377);
#15308=AXIS2_PLACEMENT_3D('',#21361,#17379,#17380);
#15309=AXIS2_PLACEMENT_3D('',#21362,#17381,#17382);
#15310=AXIS2_PLACEMENT_3D('',#21364,#17383,#17384);
#15311=AXIS2_PLACEMENT_3D('',#21366,#17386,#17387);
#15312=AXIS2_PLACEMENT_3D('',#21370,#17390,#17391);
#15313=AXIS2_PLACEMENT_3D('',#21371,#17392,#17393);
#15314=AXIS2_PLACEMENT_3D('',#21372,#17394,#17395);
#15315=AXIS2_PLACEMENT_3D('',#21374,#17397,#17398);
#15316=AXIS2_PLACEMENT_3D('',#21376,#17400,#17401);
#15317=AXIS2_PLACEMENT_3D('',#21377,#17402,#17403);
#15318=AXIS2_PLACEMENT_3D('',#21379,#17405,#17406);
#15319=AXIS2_PLACEMENT_3D('',#21381,#17408,#17409);
#15320=AXIS2_PLACEMENT_3D('',#21382,#17410,#17411);
#15321=AXIS2_PLACEMENT_3D('',#21384,#17413,#17414);
#15322=AXIS2_PLACEMENT_3D('',#21385,#17415,#17416);
#15323=AXIS2_PLACEMENT_3D('',#21386,#17417,#17418);
#15324=AXIS2_PLACEMENT_3D('',#21387,#17419,#17420);
#15325=AXIS2_PLACEMENT_3D('',#21389,#17421,#17422);
#15326=AXIS2_PLACEMENT_3D('',#21392,#17424,#17425);
#15327=AXIS2_PLACEMENT_3D('',#21393,#17426,#17427);
#15328=AXIS2_PLACEMENT_3D('',#21395,#17428,#17429);
#15329=AXIS2_PLACEMENT_3D('',#21397,#17431,#17432);
#15330=AXIS2_PLACEMENT_3D('',#21402,#17434,#17435);
#15331=AXIS2_PLACEMENT_3D('',#21406,#17437,#17438);
#15332=AXIS2_PLACEMENT_3D('',#21410,#17440,#17441);
#15333=AXIS2_PLACEMENT_3D('',#21413,#17443,#17444);
#15334=AXIS2_PLACEMENT_3D('',#21415,#17445,#17446);
#15335=AXIS2_PLACEMENT_3D('',#21417,#17447,#17448);
#15336=AXIS2_PLACEMENT_3D('',#21418,#17449,#17450);
#15337=AXIS2_PLACEMENT_3D('',#21420,#17451,#17452);
#15338=AXIS2_PLACEMENT_3D('',#21422,#17454,#17455);
#15339=AXIS2_PLACEMENT_3D('',#21427,#17457,#17458);
#15340=AXIS2_PLACEMENT_3D('',#21431,#17460,#17461);
#15341=AXIS2_PLACEMENT_3D('',#21435,#17463,#17464);
#15342=AXIS2_PLACEMENT_3D('',#21438,#17466,#17467);
#15343=AXIS2_PLACEMENT_3D('',#21440,#17468,#17469);
#15344=AXIS2_PLACEMENT_3D('',#21442,#17470,#17471);
#15345=AXIS2_PLACEMENT_3D('',#21443,#17472,#17473);
#15346=AXIS2_PLACEMENT_3D('',#21449,#17477,#17478);
#15347=AXIS2_PLACEMENT_3D('',#21451,#17479,#17480);
#15348=AXIS2_PLACEMENT_3D('',#21453,#17482,#17483);
#15349=AXIS2_PLACEMENT_3D('',#21457,#17486,#17487);
#15350=AXIS2_PLACEMENT_3D('',#21459,#17488,#17489);
#15351=AXIS2_PLACEMENT_3D('',#21461,#17491,#17492);
#15352=AXIS2_PLACEMENT_3D('',#21465,#17495,#17496);
#15353=AXIS2_PLACEMENT_3D('',#21467,#17497,#17498);
#15354=AXIS2_PLACEMENT_3D('',#21469,#17500,#17501);
#15355=AXIS2_PLACEMENT_3D('',#21473,#17504,#17505);
#15356=AXIS2_PLACEMENT_3D('',#21474,#17506,#17507);
#15357=AXIS2_PLACEMENT_3D('',#21475,#17508,#17509);
#15358=AXIS2_PLACEMENT_3D('',#21479,#17511,#17512);
#15359=AXIS2_PLACEMENT_3D('',#21481,#17514,#17515);
#15360=AXIS2_PLACEMENT_3D('',#21485,#17518,#17519);
#15361=AXIS2_PLACEMENT_3D('',#21488,#17521,#17522);
#15362=AXIS2_PLACEMENT_3D('',#21489,#17523,#17524);
#15363=AXIS2_PLACEMENT_3D('',#21493,#17527,#17528);
#15364=AXIS2_PLACEMENT_3D('',#21501,#17533,#17534);
#15365=AXIS2_PLACEMENT_3D('',#21504,#17536,#17537);
#15366=AXIS2_PLACEMENT_3D('',#21505,#17538,#17539);
#15367=AXIS2_PLACEMENT_3D('',#21509,#17542,#17543);
#15368=AXIS2_PLACEMENT_3D('',#21512,#17545,#17546);
#15369=AXIS2_PLACEMENT_3D('',#21513,#17547,#17548);
#15370=AXIS2_PLACEMENT_3D('',#21517,#17551,#17552);
#15371=AXIS2_PLACEMENT_3D('',#21521,#17554,#17555);
#15372=AXIS2_PLACEMENT_3D('',#21522,#17556,#17557);
#15373=AXIS2_PLACEMENT_3D('',#21523,#17558,#17559);
#15374=AXIS2_PLACEMENT_3D('',#21529,#17563,#17564);
#15375=AXIS2_PLACEMENT_3D('',#21530,#17565,#17566);
#15376=AXIS2_PLACEMENT_3D('',#21531,#17567,#17568);
#15377=AXIS2_PLACEMENT_3D('',#21532,#17569,#17570);
#15378=AXIS2_PLACEMENT_3D('',#21536,#17572,#17573);
#15379=AXIS2_PLACEMENT_3D('',#21538,#17575,#17576);
#15380=AXIS2_PLACEMENT_3D('',#21542,#17579,#17580);
#15381=AXIS2_PLACEMENT_3D('',#21545,#17582,#17583);
#15382=AXIS2_PLACEMENT_3D('',#21546,#17584,#17585);
#15383=AXIS2_PLACEMENT_3D('',#21550,#17588,#17589);
#15384=AXIS2_PLACEMENT_3D('',#21552,#17591,#17592);
#15385=AXIS2_PLACEMENT_3D('',#21555,#17595,#17596);
#15386=AXIS2_PLACEMENT_3D('',#21557,#17598,#17599);
#15387=AXIS2_PLACEMENT_3D('',#21559,#17601,#17602);
#15388=AXIS2_PLACEMENT_3D('',#21561,#17604,#17605);
#15389=AXIS2_PLACEMENT_3D('',#21565,#17608,#17609);
#15390=AXIS2_PLACEMENT_3D('',#21568,#17611,#17612);
#15391=AXIS2_PLACEMENT_3D('',#21569,#17613,#17614);
#15392=AXIS2_PLACEMENT_3D('',#21573,#17617,#17618);
#15393=AXIS2_PLACEMENT_3D('',#21574,#17619,#17620);
#15394=AXIS2_PLACEMENT_3D('',#21575,#17621,#17622);
#15395=AXIS2_PLACEMENT_3D('',#21578,#17625,#17626);
#15396=AXIS2_PLACEMENT_3D('',#21580,#17628,#17629);
#15397=AXIS2_PLACEMENT_3D('',#21581,#17630,#17631);
#15398=AXIS2_PLACEMENT_3D('',#21582,#17632,#17633);
#15399=AXIS2_PLACEMENT_3D('',#21584,#17635,#17636);
#15400=AXIS2_PLACEMENT_3D('',#21586,#17638,#17639);
#15401=AXIS2_PLACEMENT_3D('',#21588,#17641,#17642);
#15402=AXIS2_PLACEMENT_3D('',#21590,#17644,#17645);
#15403=AXIS2_PLACEMENT_3D('',#21591,#17646,#17647);
#15404=AXIS2_PLACEMENT_3D('',#21592,#17648,#17649);
#15405=AXIS2_PLACEMENT_3D('',#21601,#17654,#17655);
#15406=AXIS2_PLACEMENT_3D('',#21607,#17659,#17660);
#15407=AXIS2_PLACEMENT_3D('',#21613,#17664,#17665);
#15408=AXIS2_PLACEMENT_3D('',#21616,#17668,#17669);
#15409=AXIS2_PLACEMENT_3D('',#21617,#17670,#17671);
#15410=AXIS2_PLACEMENT_3D('',#21626,#17676,#17677);
#15411=AXIS2_PLACEMENT_3D('',#21632,#17681,#17682);
#15412=AXIS2_PLACEMENT_3D('',#21638,#17686,#17687);
#15413=AXIS2_PLACEMENT_3D('',#21641,#17690,#17691);
#15414=AXIS2_PLACEMENT_3D('',#21642,#17692,#17693);
#15415=AXIS2_PLACEMENT_3D('',#21651,#17698,#17699);
#15416=AXIS2_PLACEMENT_3D('',#21657,#17703,#17704);
#15417=AXIS2_PLACEMENT_3D('',#21663,#17708,#17709);
#15418=AXIS2_PLACEMENT_3D('',#21666,#17712,#17713);
#15419=AXIS2_PLACEMENT_3D('',#21667,#17714,#17715);
#15420=AXIS2_PLACEMENT_3D('',#21676,#17720,#17721);
#15421=AXIS2_PLACEMENT_3D('',#21682,#17725,#17726);
#15422=AXIS2_PLACEMENT_3D('',#21688,#17730,#17731);
#15423=AXIS2_PLACEMENT_3D('',#21691,#17734,#17735);
#15424=AXIS2_PLACEMENT_3D('',#21692,#17736,#17737);
#15425=AXIS2_PLACEMENT_3D('',#21693,#17738,#17739);
#15426=AXIS2_PLACEMENT_3D('',#21694,#17740,#17741);
#15427=AXIS2_PLACEMENT_3D('',#21701,#17745,#17746);
#15428=AXIS2_PLACEMENT_3D('',#21708,#17750,#17751);
#15429=AXIS2_PLACEMENT_3D('',#21715,#17755,#17756);
#15430=AXIS2_PLACEMENT_3D('',#21722,#17760,#17761);
#15431=AXIS2_PLACEMENT_3D('',#21729,#17765,#17766);
#15432=AXIS2_PLACEMENT_3D('',#21736,#17770,#17771);
#15433=AXIS2_PLACEMENT_3D('',#21743,#17775,#17776);
#15434=AXIS2_PLACEMENT_3D('',#21746,#17779,#17780);
#15435=AXIS2_PLACEMENT_3D('',#21753,#17784,#17785);
#15436=AXIS2_PLACEMENT_3D('',#21756,#17788,#17789);
#15437=AXIS2_PLACEMENT_3D('',#21759,#17792,#17793);
#15438=AXIS2_PLACEMENT_3D('',#21762,#17796,#17797);
#15439=AXIS2_PLACEMENT_3D('',#21765,#17800,#17801);
#15440=AXIS2_PLACEMENT_3D('',#21768,#17804,#17805);
#15441=AXIS2_PLACEMENT_3D('',#21771,#17808,#17809);
#15442=AXIS2_PLACEMENT_3D('',#21774,#17812,#17813);
#15443=AXIS2_PLACEMENT_3D('',#21777,#17816,#17817);
#15444=AXIS2_PLACEMENT_3D('',#21780,#17820,#17821);
#15445=AXIS2_PLACEMENT_3D('',#21783,#17824,#17825);
#15446=AXIS2_PLACEMENT_3D('',#21786,#17828,#17829);
#15447=AXIS2_PLACEMENT_3D('',#21787,#17830,#17831);
#15448=AXIS2_PLACEMENT_3D('',#21788,#17832,#17833);
#15449=AXIS2_PLACEMENT_3D('',#21790,#17834,#17835);
#15450=AXIS2_PLACEMENT_3D('',#21791,#17836,#17837);
#15451=AXIS2_PLACEMENT_3D('',#21792,#17838,#17839);
#15452=AXIS2_PLACEMENT_3D('',#21794,#17840,#17841);
#15453=AXIS2_PLACEMENT_3D('',#21795,#17842,#17843);
#15454=AXIS2_PLACEMENT_3D('',#21796,#17844,#17845);
#15455=AXIS2_PLACEMENT_3D('',#21798,#17847,#17848);
#15456=AXIS2_PLACEMENT_3D('',#21799,#17849,#17850);
#15457=AXIS2_PLACEMENT_3D('',#21815,#17852,#17853);
#15458=AXIS2_PLACEMENT_3D('',#21823,#17854,#17855);
#15459=AXIS2_PLACEMENT_3D('',#21871,#17857,#17858);
#15460=AXIS2_PLACEMENT_3D('',#21919,#17860,#17861);
#15461=AXIS2_PLACEMENT_3D('',#21973,#17863,#17864);
#15462=AXIS2_PLACEMENT_3D('',#22021,#17866,#17867);
#15463=AXIS2_PLACEMENT_3D('',#22069,#17869,#17870);
#15464=AXIS2_PLACEMENT_3D('',#22123,#17872,#17873);
#15465=AXIS2_PLACEMENT_3D('',#22171,#17875,#17876);
#15466=AXIS2_PLACEMENT_3D('',#22219,#17878,#17879);
#15467=AXIS2_PLACEMENT_3D('',#22267,#17881,#17882);
#15468=AXIS2_PLACEMENT_3D('',#22321,#17884,#17885);
#15469=AXIS2_PLACEMENT_3D('',#22369,#17887,#17888);
#15470=AXIS2_PLACEMENT_3D('',#22417,#17890,#17891);
#15471=AXIS2_PLACEMENT_3D('',#22471,#17893,#17894);
#15472=AXIS2_PLACEMENT_3D('',#22519,#17896,#17897);
#15473=AXIS2_PLACEMENT_3D('',#22567,#17899,#17900);
#15474=AXIS2_PLACEMENT_3D('',#22621,#17902,#17903);
#15475=AXIS2_PLACEMENT_3D('',#22669,#17905,#17906);
#15476=AXIS2_PLACEMENT_3D('',#22717,#17908,#17909);
#15477=AXIS2_PLACEMENT_3D('',#22771,#17911,#17912);
#15478=AXIS2_PLACEMENT_3D('',#22819,#17914,#17915);
#15479=AXIS2_PLACEMENT_3D('',#22867,#17917,#17918);
#15480=AXIS2_PLACEMENT_3D('',#22921,#17920,#17921);
#15481=AXIS2_PLACEMENT_3D('',#22969,#17923,#17924);
#15482=AXIS2_PLACEMENT_3D('',#23017,#17926,#17927);
#15483=AXIS2_PLACEMENT_3D('',#23071,#17929,#17930);
#15484=AXIS2_PLACEMENT_3D('',#23119,#17932,#17933);
#15485=AXIS2_PLACEMENT_3D('',#23167,#17935,#17936);
#15486=AXIS2_PLACEMENT_3D('',#23182,#17938,#17939);
#15487=AXIS2_PLACEMENT_3D('',#23191,#17940,#17941);
#15488=AXIS2_PLACEMENT_3D('',#23215,#17943,#17944);
#15489=AXIS2_PLACEMENT_3D('',#23240,#17946,#17947);
#15490=AXIS2_PLACEMENT_3D('',#23265,#17949,#17950);
#15491=AXIS2_PLACEMENT_3D('',#23289,#17952,#17953);
#15492=AXIS2_PLACEMENT_3D('',#23314,#17955,#17956);
#15493=AXIS2_PLACEMENT_3D('',#23339,#17958,#17959);
#15494=AXIS2_PLACEMENT_3D('',#23363,#17961,#17962);
#15495=AXIS2_PLACEMENT_3D('',#23388,#17964,#17965);
#15496=AXIS2_PLACEMENT_3D('',#23413,#17967,#17968);
#15497=AXIS2_PLACEMENT_3D('',#23437,#17970,#17971);
#15498=AXIS2_PLACEMENT_3D('',#23462,#17973,#17974);
#15499=AXIS2_PLACEMENT_3D('',#23487,#17976,#17977);
#15500=AXIS2_PLACEMENT_3D('',#23511,#17979,#17980);
#15501=AXIS2_PLACEMENT_3D('',#23536,#17982,#17983);
#15502=AXIS2_PLACEMENT_3D('',#23561,#17985,#17986);
#15503=AXIS2_PLACEMENT_3D('',#23585,#17988,#17989);
#15504=AXIS2_PLACEMENT_3D('',#23610,#17991,#17992);
#15505=AXIS2_PLACEMENT_3D('',#23635,#17994,#17995);
#15506=AXIS2_PLACEMENT_3D('',#23659,#17997,#17998);
#15507=AXIS2_PLACEMENT_3D('',#23683,#18000,#18001);
#15508=AXIS2_PLACEMENT_3D('',#23708,#18003,#18004);
#15509=AXIS2_PLACEMENT_3D('',#23733,#18006,#18007);
#15510=AXIS2_PLACEMENT_3D('',#23757,#18009,#18010);
#15511=AXIS2_PLACEMENT_3D('',#23782,#18012,#18013);
#15512=AXIS2_PLACEMENT_3D('',#23807,#18015,#18016);
#15513=AXIS2_PLACEMENT_3D('',#23831,#18018,#18019);
#15514=AXIS2_PLACEMENT_3D('',#23834,#18020,#18021);
#15515=AXIS2_PLACEMENT_3D('',#23837,#18023,#18024);
#15516=AXIS2_PLACEMENT_3D('',#23839,#18025,#18026);
#15517=AXIS2_PLACEMENT_3D('',#23841,#18027,#18028);
#15518=AXIS2_PLACEMENT_3D('',#23843,#18029,#18030);
#15519=AXIS2_PLACEMENT_3D('',#23845,#18031,#18032);
#15520=AXIS2_PLACEMENT_3D('',#23847,#18033,#18034);
#15521=AXIS2_PLACEMENT_3D('',#23849,#18035,#18036);
#15522=AXIS2_PLACEMENT_3D('',#23851,#18037,#18038);
#15523=AXIS2_PLACEMENT_3D('',#23853,#18039,#18040);
#15524=AXIS2_PLACEMENT_3D('',#23855,#18041,#18042);
#15525=AXIS2_PLACEMENT_3D('',#23857,#18043,#18044);
#15526=AXIS2_PLACEMENT_3D('',#23859,#18045,#18046);
#15527=AXIS2_PLACEMENT_3D('',#23861,#18047,#18048);
#15528=AXIS2_PLACEMENT_3D('',#23863,#18049,#18050);
#15529=AXIS2_PLACEMENT_3D('',#23865,#18051,#18052);
#15530=AXIS2_PLACEMENT_3D('',#23867,#18053,#18054);
#15531=AXIS2_PLACEMENT_3D('',#23869,#18055,#18056);
#15532=AXIS2_PLACEMENT_3D('',#23871,#18057,#18058);
#15533=AXIS2_PLACEMENT_3D('',#23873,#18059,#18060);
#15534=AXIS2_PLACEMENT_3D('',#23875,#18061,#18062);
#15535=AXIS2_PLACEMENT_3D('',#23877,#18063,#18064);
#15536=AXIS2_PLACEMENT_3D('',#23879,#18065,#18066);
#15537=AXIS2_PLACEMENT_3D('',#23881,#18067,#18068);
#15538=AXIS2_PLACEMENT_3D('',#23883,#18069,#18070);
#15539=AXIS2_PLACEMENT_3D('',#23885,#18071,#18072);
#15540=AXIS2_PLACEMENT_3D('',#23887,#18073,#18074);
#15541=AXIS2_PLACEMENT_3D('',#23889,#18075,#18076);
#15542=AXIS2_PLACEMENT_3D('',#23891,#18077,#18078);
#15543=AXIS2_PLACEMENT_3D('',#23893,#18079,#18080);
#15544=AXIS2_PLACEMENT_3D('',#23895,#18081,#18082);
#15545=AXIS2_PLACEMENT_3D('',#23897,#18083,#18084);
#15546=AXIS2_PLACEMENT_3D('',#23899,#18085,#18086);
#15547=AXIS2_PLACEMENT_3D('',#23901,#18087,#18088);
#15548=AXIS2_PLACEMENT_3D('',#23903,#18089,#18090);
#15549=AXIS2_PLACEMENT_3D('',#23905,#18091,#18092);
#15550=AXIS2_PLACEMENT_3D('',#23907,#18093,#18094);
#15551=AXIS2_PLACEMENT_3D('',#23909,#18095,#18096);
#15552=AXIS2_PLACEMENT_3D('',#23911,#18097,#18098);
#15553=AXIS2_PLACEMENT_3D('',#23913,#18099,#18100);
#15554=AXIS2_PLACEMENT_3D('',#23915,#18101,#18102);
#15555=AXIS2_PLACEMENT_3D('',#23917,#18103,#18104);
#15556=AXIS2_PLACEMENT_3D('',#23919,#18105,#18106);
#15557=AXIS2_PLACEMENT_3D('',#23921,#18107,#18108);
#15558=AXIS2_PLACEMENT_3D('',#23923,#18109,#18110);
#15559=AXIS2_PLACEMENT_3D('',#23925,#18111,#18112);
#15560=AXIS2_PLACEMENT_3D('',#23927,#18113,#18114);
#15561=AXIS2_PLACEMENT_3D('',#23929,#18115,#18116);
#15562=AXIS2_PLACEMENT_3D('',#23931,#18117,#18118);
#15563=AXIS2_PLACEMENT_3D('',#23932,#18119,#18120);
#15564=AXIS2_PLACEMENT_3D('',#23933,#18121,#18122);
#15565=AXIS2_PLACEMENT_3D('',#23935,#18123,#18124);
#15566=AXIS2_PLACEMENT_3D('',#23939,#18126,#18127);
#15567=AXIS2_PLACEMENT_3D('',#23944,#18130,#18131);
#15568=AXIS2_PLACEMENT_3D('',#23949,#18134,#18135);
#15569=AXIS2_PLACEMENT_3D('',#23954,#18138,#18139);
#15570=AXIS2_PLACEMENT_3D('',#23959,#18142,#18143);
#15571=AXIS2_PLACEMENT_3D('',#23964,#18146,#18147);
#15572=AXIS2_PLACEMENT_3D('',#23969,#18150,#18151);
#15573=AXIS2_PLACEMENT_3D('',#23974,#18154,#18155);
#15574=AXIS2_PLACEMENT_3D('',#23979,#18158,#18159);
#15575=AXIS2_PLACEMENT_3D('',#23984,#18162,#18163);
#15576=AXIS2_PLACEMENT_3D('',#23989,#18166,#18167);
#15577=AXIS2_PLACEMENT_3D('',#23994,#18170,#18171);
#15578=AXIS2_PLACEMENT_3D('',#23999,#18174,#18175);
#15579=AXIS2_PLACEMENT_3D('',#24004,#18178,#18179);
#15580=AXIS2_PLACEMENT_3D('',#24009,#18182,#18183);
#15581=AXIS2_PLACEMENT_3D('',#24014,#18186,#18187);
#15582=AXIS2_PLACEMENT_3D('',#24019,#18190,#18191);
#15583=AXIS2_PLACEMENT_3D('',#24024,#18194,#18195);
#15584=AXIS2_PLACEMENT_3D('',#24029,#18198,#18199);
#15585=AXIS2_PLACEMENT_3D('',#24034,#18202,#18203);
#15586=AXIS2_PLACEMENT_3D('',#24039,#18206,#18207);
#15587=AXIS2_PLACEMENT_3D('',#24044,#18210,#18211);
#15588=AXIS2_PLACEMENT_3D('',#24049,#18214,#18215);
#15589=AXIS2_PLACEMENT_3D('',#24054,#18218,#18219);
#15590=AXIS2_PLACEMENT_3D('',#24058,#18222,#18223);
#15591=AXIS2_PLACEMENT_3D('',#24059,#18224,#18225);
#15592=AXIS2_PLACEMENT_3D('',#24062,#18226,#18227);
#15593=AXIS2_PLACEMENT_3D('',#25090,#18228,#18229);
#15594=AXIS2_PLACEMENT_3D('',#25092,#18230,#18231);
#15595=AXIS2_PLACEMENT_3D('',#25093,#18232,#18233);
#15596=AXIS2_PLACEMENT_3D('',#25192,#18234,#18235);
#15597=AXIS2_PLACEMENT_3D('',#25193,#18236,#18237);
#15598=AXIS2_PLACEMENT_3D('',#25925,#18238,#18239);
#15599=AXIS2_PLACEMENT_3D('',#25931,#18243,#18244);
#15600=AXIS2_PLACEMENT_3D('',#25933,#18246,#18247);
#15601=AXIS2_PLACEMENT_3D('',#25935,#18249,#18250);
#15602=AXIS2_PLACEMENT_3D('',#25936,#18251,#18252);
#15603=AXIS2_PLACEMENT_3D('',#25942,#18256,#18257);
#15604=AXIS2_PLACEMENT_3D('',#25944,#18259,#18260);
#15605=AXIS2_PLACEMENT_3D('',#25946,#18262,#18263);
#15606=AXIS2_PLACEMENT_3D('',#25947,#18264,#18265);
#15607=AXIS2_PLACEMENT_3D('',#25953,#18269,#18270);
#15608=AXIS2_PLACEMENT_3D('',#25955,#18272,#18273);
#15609=AXIS2_PLACEMENT_3D('',#25957,#18275,#18276);
#15610=AXIS2_PLACEMENT_3D('',#25958,#18277,#18278);
#15611=AXIS2_PLACEMENT_3D('',#25964,#18282,#18283);
#15612=AXIS2_PLACEMENT_3D('',#25966,#18285,#18286);
#15613=AXIS2_PLACEMENT_3D('',#25968,#18288,#18289);
#15614=AXIS2_PLACEMENT_3D('',#25969,#18290,#18291);
#15615=AXIS2_PLACEMENT_3D('',#25975,#18295,#18296);
#15616=AXIS2_PLACEMENT_3D('',#25977,#18298,#18299);
#15617=AXIS2_PLACEMENT_3D('',#25979,#18301,#18302);
#15618=AXIS2_PLACEMENT_3D('',#25980,#18303,#18304);
#15619=AXIS2_PLACEMENT_3D('',#25986,#18308,#18309);
#15620=AXIS2_PLACEMENT_3D('',#25988,#18311,#18312);
#15621=AXIS2_PLACEMENT_3D('',#25990,#18314,#18315);
#15622=AXIS2_PLACEMENT_3D('',#25991,#18316,#18317);
#15623=AXIS2_PLACEMENT_3D('',#25997,#18321,#18322);
#15624=AXIS2_PLACEMENT_3D('',#25999,#18324,#18325);
#15625=AXIS2_PLACEMENT_3D('',#26001,#18327,#18328);
#15626=AXIS2_PLACEMENT_3D('',#26002,#18329,#18330);
#15627=AXIS2_PLACEMENT_3D('',#26008,#18334,#18335);
#15628=AXIS2_PLACEMENT_3D('',#26010,#18337,#18338);
#15629=AXIS2_PLACEMENT_3D('',#26012,#18340,#18341);
#15630=AXIS2_PLACEMENT_3D('',#26013,#18342,#18343);
#15631=AXIS2_PLACEMENT_3D('',#26019,#18347,#18348);
#15632=AXIS2_PLACEMENT_3D('',#26021,#18350,#18351);
#15633=AXIS2_PLACEMENT_3D('',#26023,#18353,#18354);
#15634=AXIS2_PLACEMENT_3D('',#26024,#18355,#18356);
#15635=AXIS2_PLACEMENT_3D('',#26030,#18360,#18361);
#15636=AXIS2_PLACEMENT_3D('',#26032,#18363,#18364);
#15637=AXIS2_PLACEMENT_3D('',#26034,#18366,#18367);
#15638=AXIS2_PLACEMENT_3D('',#26035,#18368,#18369);
#15639=AXIS2_PLACEMENT_3D('',#26041,#18373,#18374);
#15640=AXIS2_PLACEMENT_3D('',#26043,#18376,#18377);
#15641=AXIS2_PLACEMENT_3D('',#26045,#18379,#18380);
#15642=AXIS2_PLACEMENT_3D('',#26046,#18381,#18382);
#15643=AXIS2_PLACEMENT_3D('',#26052,#18386,#18387);
#15644=AXIS2_PLACEMENT_3D('',#26054,#18389,#18390);
#15645=AXIS2_PLACEMENT_3D('',#26056,#18392,#18393);
#15646=AXIS2_PLACEMENT_3D('',#26057,#18394,#18395);
#15647=AXIS2_PLACEMENT_3D('',#26063,#18399,#18400);
#15648=AXIS2_PLACEMENT_3D('',#26065,#18402,#18403);
#15649=AXIS2_PLACEMENT_3D('',#26067,#18405,#18406);
#15650=AXIS2_PLACEMENT_3D('',#26068,#18407,#18408);
#15651=AXIS2_PLACEMENT_3D('',#26074,#18412,#18413);
#15652=AXIS2_PLACEMENT_3D('',#26076,#18415,#18416);
#15653=AXIS2_PLACEMENT_3D('',#26078,#18418,#18419);
#15654=AXIS2_PLACEMENT_3D('',#26079,#18420,#18421);
#15655=AXIS2_PLACEMENT_3D('',#26085,#18425,#18426);
#15656=AXIS2_PLACEMENT_3D('',#26087,#18428,#18429);
#15657=AXIS2_PLACEMENT_3D('',#26089,#18431,#18432);
#15658=AXIS2_PLACEMENT_3D('',#26090,#18433,#18434);
#15659=AXIS2_PLACEMENT_3D('',#26096,#18438,#18439);
#15660=AXIS2_PLACEMENT_3D('',#26098,#18441,#18442);
#15661=AXIS2_PLACEMENT_3D('',#26100,#18444,#18445);
#15662=AXIS2_PLACEMENT_3D('',#26101,#18446,#18447);
#15663=AXIS2_PLACEMENT_3D('',#26107,#18451,#18452);
#15664=AXIS2_PLACEMENT_3D('',#26109,#18454,#18455);
#15665=AXIS2_PLACEMENT_3D('',#26111,#18457,#18458);
#15666=AXIS2_PLACEMENT_3D('',#26112,#18459,#18460);
#15667=AXIS2_PLACEMENT_3D('',#26118,#18464,#18465);
#15668=AXIS2_PLACEMENT_3D('',#26120,#18467,#18468);
#15669=AXIS2_PLACEMENT_3D('',#26122,#18470,#18471);
#15670=AXIS2_PLACEMENT_3D('',#26123,#18472,#18473);
#15671=AXIS2_PLACEMENT_3D('',#26129,#18477,#18478);
#15672=AXIS2_PLACEMENT_3D('',#26131,#18480,#18481);
#15673=AXIS2_PLACEMENT_3D('',#26133,#18483,#18484);
#15674=AXIS2_PLACEMENT_3D('',#26134,#18485,#18486);
#15675=AXIS2_PLACEMENT_3D('',#26140,#18490,#18491);
#15676=AXIS2_PLACEMENT_3D('',#26142,#18493,#18494);
#15677=AXIS2_PLACEMENT_3D('',#26144,#18496,#18497);
#15678=AXIS2_PLACEMENT_3D('',#26145,#18498,#18499);
#15679=AXIS2_PLACEMENT_3D('',#26151,#18503,#18504);
#15680=AXIS2_PLACEMENT_3D('',#26153,#18506,#18507);
#15681=AXIS2_PLACEMENT_3D('',#26155,#18509,#18510);
#15682=AXIS2_PLACEMENT_3D('',#26156,#18511,#18512);
#15683=AXIS2_PLACEMENT_3D('',#26162,#18516,#18517);
#15684=AXIS2_PLACEMENT_3D('',#26164,#18519,#18520);
#15685=AXIS2_PLACEMENT_3D('',#26166,#18522,#18523);
#15686=AXIS2_PLACEMENT_3D('',#26167,#18524,#18525);
#15687=AXIS2_PLACEMENT_3D('',#26173,#18529,#18530);
#15688=AXIS2_PLACEMENT_3D('',#26175,#18532,#18533);
#15689=AXIS2_PLACEMENT_3D('',#26177,#18535,#18536);
#15690=AXIS2_PLACEMENT_3D('',#26178,#18537,#18538);
#15691=AXIS2_PLACEMENT_3D('',#26184,#18542,#18543);
#15692=AXIS2_PLACEMENT_3D('',#26186,#18545,#18546);
#15693=AXIS2_PLACEMENT_3D('',#26188,#18548,#18549);
#15694=AXIS2_PLACEMENT_3D('',#26189,#18550,#18551);
#15695=AXIS2_PLACEMENT_3D('',#26191,#18552,#18553);
#15696=AXIS2_PLACEMENT_3D('',#26192,#18554,#18555);
#15697=AXIS2_PLACEMENT_3D('',#26194,#18557,#18558);
#15698=AXIS2_PLACEMENT_3D('',#26195,#18559,#18560);
#15699=AXIS2_PLACEMENT_3D('',#26197,#18561,#18562);
#15700=AXIS2_PLACEMENT_3D('',#26199,#18564,#18565);
#15701=AXIS2_PLACEMENT_3D('',#26201,#18566,#18567);
#15702=AXIS2_PLACEMENT_3D('',#26202,#18568,#18569);
#15703=AXIS2_PLACEMENT_3D('',#26205,#18571,#18572);
#15704=AXIS2_PLACEMENT_3D('',#26206,#18573,#18574);
#15705=AXIS2_PLACEMENT_3D('',#26207,#18575,#18576);
#15706=AXIS2_PLACEMENT_3D('',#26208,#18577,#18578);
#15707=AXIS2_PLACEMENT_3D('',#26211,#18579,#18580);
#15708=AXIS2_PLACEMENT_3D('',#26212,#18581,#18582);
#15709=AXIS2_PLACEMENT_3D('',#26215,#18584,#18585);
#15710=AXIS2_PLACEMENT_3D('',#26216,#18586,#18587);
#15711=AXIS2_PLACEMENT_3D('',#26219,#18589,#18590);
#15712=AXIS2_PLACEMENT_3D('',#26220,#18591,#18592);
#15713=AXIS2_PLACEMENT_3D('',#26222,#18593,#18594);
#15714=AXIS2_PLACEMENT_3D('',#26223,#18595,#18596);
#15715=AXIS2_PLACEMENT_3D('',#26234,#18600,#18601);
#15716=AXIS2_PLACEMENT_3D('',#26236,#18602,#18603);
#15717=AXIS2_PLACEMENT_3D('',#26238,#18604,#18605);
#15718=AXIS2_PLACEMENT_3D('',#26247,#18607,#18608);
#15719=AXIS2_PLACEMENT_3D('',#26256,#18610,#18611);
#15720=AXIS2_PLACEMENT_3D('',#26260,#18613,#18614);
#15721=AXIS2_PLACEMENT_3D('',#26264,#18616,#18617);
#15722=AXIS2_PLACEMENT_3D('',#26268,#18619,#18620);
#15723=AXIS2_PLACEMENT_3D('',#26272,#18622,#18623);
#15724=AXIS2_PLACEMENT_3D('',#26276,#18625,#18626);
#15725=AXIS2_PLACEMENT_3D('',#26280,#18628,#18629);
#15726=AXIS2_PLACEMENT_3D('',#26284,#18631,#18632);
#15727=AXIS2_PLACEMENT_3D('',#26288,#18634,#18635);
#15728=AXIS2_PLACEMENT_3D('',#26292,#18637,#18638);
#15729=AXIS2_PLACEMENT_3D('',#26296,#18640,#18641);
#15730=AXIS2_PLACEMENT_3D('',#26300,#18643,#18644);
#15731=AXIS2_PLACEMENT_3D('',#26304,#18646,#18647);
#15732=AXIS2_PLACEMENT_3D('',#26308,#18649,#18650);
#15733=AXIS2_PLACEMENT_3D('',#26311,#18652,#18653);
#15734=AXIS2_PLACEMENT_3D('',#26313,#18654,#18655);
#15735=AXIS2_PLACEMENT_3D('',#26317,#18657,#18658);
#15736=AXIS2_PLACEMENT_3D('',#26321,#18660,#18661);
#15737=AXIS2_PLACEMENT_3D('',#26325,#18663,#18664);
#15738=AXIS2_PLACEMENT_3D('',#26329,#18666,#18667);
#15739=AXIS2_PLACEMENT_3D('',#26333,#18669,#18670);
#15740=AXIS2_PLACEMENT_3D('',#26337,#18672,#18673);
#15741=AXIS2_PLACEMENT_3D('',#26341,#18675,#18676);
#15742=AXIS2_PLACEMENT_3D('',#26345,#18678,#18679);
#15743=AXIS2_PLACEMENT_3D('',#26349,#18681,#18682);
#15744=AXIS2_PLACEMENT_3D('',#26353,#18684,#18685);
#15745=AXIS2_PLACEMENT_3D('',#26357,#18687,#18688);
#15746=AXIS2_PLACEMENT_3D('',#26361,#18690,#18691);
#15747=AXIS2_PLACEMENT_3D('',#26365,#18693,#18694);
#15748=AXIS2_PLACEMENT_3D('',#26369,#18696,#18697);
#15749=AXIS2_PLACEMENT_3D('',#26373,#18699,#18700);
#15750=AXIS2_PLACEMENT_3D('',#26375,#18702,#18703);
#15751=AXIS2_PLACEMENT_3D('',#26655,#18705,#18706);
#15752=AXIS2_PLACEMENT_3D('',#26659,#18709,#18710);
#15753=AXIS2_PLACEMENT_3D('',#26663,#18713,#18714);
#15754=AXIS2_PLACEMENT_3D('',#26667,#18717,#18718);
#15755=AXIS2_PLACEMENT_3D('',#26671,#18721,#18722);
#15756=AXIS2_PLACEMENT_3D('',#26675,#18725,#18726);
#15757=AXIS2_PLACEMENT_3D('',#26679,#18729,#18730);
#15758=AXIS2_PLACEMENT_3D('',#26683,#18733,#18734);
#15759=AXIS2_PLACEMENT_3D('',#26687,#18737,#18738);
#15760=AXIS2_PLACEMENT_3D('',#26691,#18741,#18742);
#15761=AXIS2_PLACEMENT_3D('',#26695,#18745,#18746);
#15762=AXIS2_PLACEMENT_3D('',#26699,#18749,#18750);
#15763=AXIS2_PLACEMENT_3D('',#26703,#18753,#18754);
#15764=AXIS2_PLACEMENT_3D('',#26707,#18757,#18758);
#15765=AXIS2_PLACEMENT_3D('',#26711,#18761,#18762);
#15766=AXIS2_PLACEMENT_3D('',#26715,#18765,#18766);
#15767=AXIS2_PLACEMENT_3D('',#26719,#18769,#18770);
#15768=AXIS2_PLACEMENT_3D('',#26723,#18773,#18774);
#15769=AXIS2_PLACEMENT_3D('',#26727,#18777,#18778);
#15770=AXIS2_PLACEMENT_3D('',#26731,#18781,#18782);
#15771=AXIS2_PLACEMENT_3D('',#26735,#18785,#18786);
#15772=AXIS2_PLACEMENT_3D('',#26739,#18789,#18790);
#15773=AXIS2_PLACEMENT_3D('',#26743,#18793,#18794);
#15774=AXIS2_PLACEMENT_3D('',#26747,#18797,#18798);
#15775=AXIS2_PLACEMENT_3D('',#26751,#18801,#18802);
#15776=AXIS2_PLACEMENT_3D('',#26755,#18805,#18806);
#15777=AXIS2_PLACEMENT_3D('',#26759,#18809,#18810);
#15778=AXIS2_PLACEMENT_3D('',#26763,#18813,#18814);
#15779=AXIS2_PLACEMENT_3D('',#26767,#18817,#18818);
#15780=AXIS2_PLACEMENT_3D('',#26851,#18821,#18822);
#15781=AXIS2_PLACEMENT_3D('',#26855,#18825,#18826);
#15782=AXIS2_PLACEMENT_3D('',#26859,#18829,#18830);
#15783=AXIS2_PLACEMENT_3D('',#26860,#18831,#18832);
#15784=AXIS2_PLACEMENT_3D('',#26861,#18833,#18834);
#15785=AXIS2_PLACEMENT_3D('',#26864,#18836,#18837);
#15786=AXIS2_PLACEMENT_3D('',#26865,#18838,#18839);
#15787=AXIS2_PLACEMENT_3D('',#26878,#18846,#18847);
#15788=AXIS2_PLACEMENT_3D('',#26887,#18852,#18853);
#15789=AXIS2_PLACEMENT_3D('',#26893,#18857,#18858);
#15790=AXIS2_PLACEMENT_3D('',#26902,#18863,#18864);
#15791=AXIS2_PLACEMENT_3D('',#26908,#18868,#18869);
#15792=AXIS2_PLACEMENT_3D('',#26911,#18872,#18873);
#15793=AXIS2_PLACEMENT_3D('',#26914,#18876,#18877);
#15794=AXIS2_PLACEMENT_3D('',#26917,#18880,#18881);
#15795=AXIS2_PLACEMENT_3D('',#26919,#18883,#18884);
#15796=AXIS2_PLACEMENT_3D('',#26921,#18886,#18887);
#15797=AXIS2_PLACEMENT_3D('',#26923,#18888,#18889);
#15798=AXIS2_PLACEMENT_3D('',#26924,#18890,#18891);
#15799=AXIS2_PLACEMENT_3D('',#26926,#18893,#18894);
#15800=AXIS2_PLACEMENT_3D('',#26928,#18896,#18897);
#15801=AXIS2_PLACEMENT_3D('',#26929,#18898,#18899);
#15802=AXIS2_PLACEMENT_3D('',#26930,#18900,#18901);
#15803=AXIS2_PLACEMENT_3D('',#26931,#18902,#18903);
#15804=AXIS2_PLACEMENT_3D('',#26932,#18904,#18905);
#15805=AXIS2_PLACEMENT_3D('',#26933,#18906,#18907);
#15806=AXIS2_PLACEMENT_3D('',#26934,#18908,#18909);
#15807=AXIS2_PLACEMENT_3D('',#26935,#18910,#18911);
#15808=AXIS2_PLACEMENT_3D('',#26936,#18912,#18913);
#15809=AXIS2_PLACEMENT_3D('',#26937,#18914,#18915);
#15810=AXIS2_PLACEMENT_3D('',#26938,#18916,#18917);
#15811=AXIS2_PLACEMENT_3D('',#26939,#18918,#18919);
#15812=AXIS2_PLACEMENT_3D('',#26940,#18920,#18921);
#15813=AXIS2_PLACEMENT_3D('',#26941,#18922,#18923);
#15814=AXIS2_PLACEMENT_3D('',#26942,#18924,#18925);
#15815=AXIS2_PLACEMENT_3D('',#26943,#18926,#18927);
#15816=AXIS2_PLACEMENT_3D('',#26944,#18928,#18929);
#15817=AXIS2_PLACEMENT_3D('',#26945,#18930,#18931);
#15818=AXIS2_PLACEMENT_3D('',#26946,#18932,#18933);
#15819=AXIS2_PLACEMENT_3D('',#26947,#18934,#18935);
#15820=AXIS2_PLACEMENT_3D('',#26948,#18936,#18937);
#15821=AXIS2_PLACEMENT_3D('',#26949,#18938,#18939);
#15822=AXIS2_PLACEMENT_3D('',#26950,#18940,#18941);
#15823=AXIS2_PLACEMENT_3D('',#26951,#18942,#18943);
#15824=AXIS2_PLACEMENT_3D('',#26952,#18944,#18945);
#15825=AXIS2_PLACEMENT_3D('',#26953,#18946,#18947);
#15826=AXIS2_PLACEMENT_3D('',#26954,#18948,#18949);
#15827=AXIS2_PLACEMENT_3D('',#26955,#18950,#18951);
#15828=AXIS2_PLACEMENT_3D('',#26956,#18952,#18953);
#15829=AXIS2_PLACEMENT_3D('',#26957,#18954,#18955);
#15830=AXIS2_PLACEMENT_3D('',#26958,#18956,#18957);
#15831=AXIS2_PLACEMENT_3D('',#26959,#18958,#18959);
#15832=AXIS2_PLACEMENT_3D('',#26960,#18960,#18961);
#15833=AXIS2_PLACEMENT_3D('',#26961,#18962,#18963);
#15834=AXIS2_PLACEMENT_3D('',#26962,#18964,#18965);
#15835=AXIS2_PLACEMENT_3D('',#26963,#18966,#18967);
#15836=AXIS2_PLACEMENT_3D('',#26964,#18968,#18969);
#15837=AXIS2_PLACEMENT_3D('',#26965,#18970,#18971);
#15838=AXIS2_PLACEMENT_3D('',#26966,#18972,#18973);
#15839=AXIS2_PLACEMENT_3D('',#26967,#18974,#18975);
#15840=AXIS2_PLACEMENT_3D('',#26968,#18976,#18977);
#15841=AXIS2_PLACEMENT_3D('',#26969,#18978,#18979);
#15842=AXIS2_PLACEMENT_3D('',#26970,#18980,#18981);
#15843=AXIS2_PLACEMENT_3D('',#26971,#18982,#18983);
#15844=AXIS2_PLACEMENT_3D('',#26972,#18984,#18985);
#15845=AXIS2_PLACEMENT_3D('',#26973,#18986,#18987);
#15846=AXIS2_PLACEMENT_3D('',#26974,#18988,#18989);
#15847=AXIS2_PLACEMENT_3D('',#26975,#18990,#18991);
#15848=AXIS2_PLACEMENT_3D('',#26977,#18993,#18994);
#15849=AXIS2_PLACEMENT_3D('',#26978,#18995,#18996);
#15850=AXIS2_PLACEMENT_3D('',#26994,#18998,#18999);
#15851=AXIS2_PLACEMENT_3D('',#27002,#19000,#19001);
#15852=AXIS2_PLACEMENT_3D('',#27050,#19003,#19004);
#15853=AXIS2_PLACEMENT_3D('',#27098,#19006,#19007);
#15854=AXIS2_PLACEMENT_3D('',#27152,#19009,#19010);
#15855=AXIS2_PLACEMENT_3D('',#27200,#19012,#19013);
#15856=AXIS2_PLACEMENT_3D('',#27248,#19015,#19016);
#15857=AXIS2_PLACEMENT_3D('',#27296,#19018,#19019);
#15858=AXIS2_PLACEMENT_3D('',#27350,#19021,#19022);
#15859=AXIS2_PLACEMENT_3D('',#27398,#19024,#19025);
#15860=AXIS2_PLACEMENT_3D('',#27446,#19027,#19028);
#15861=AXIS2_PLACEMENT_3D('',#27500,#19030,#19031);
#15862=AXIS2_PLACEMENT_3D('',#27548,#19033,#19034);
#15863=AXIS2_PLACEMENT_3D('',#27596,#19036,#19037);
#15864=AXIS2_PLACEMENT_3D('',#27650,#19039,#19040);
#15865=AXIS2_PLACEMENT_3D('',#27698,#19042,#19043);
#15866=AXIS2_PLACEMENT_3D('',#27746,#19045,#19046);
#15867=AXIS2_PLACEMENT_3D('',#27794,#19048,#19049);
#15868=AXIS2_PLACEMENT_3D('',#27845,#19051,#19052);
#15869=AXIS2_PLACEMENT_3D('',#27893,#19054,#19055);
#15870=AXIS2_PLACEMENT_3D('',#27941,#19057,#19058);
#15871=AXIS2_PLACEMENT_3D('',#27995,#19060,#19061);
#15872=AXIS2_PLACEMENT_3D('',#28043,#19063,#19064);
#15873=AXIS2_PLACEMENT_3D('',#28091,#19066,#19067);
#15874=AXIS2_PLACEMENT_3D('',#28105,#19069,#19070);
#15875=AXIS2_PLACEMENT_3D('',#28113,#19071,#19072);
#15876=AXIS2_PLACEMENT_3D('',#28137,#19074,#19075);
#15877=AXIS2_PLACEMENT_3D('',#28162,#19077,#19078);
#15878=AXIS2_PLACEMENT_3D('',#28187,#19080,#19081);
#15879=AXIS2_PLACEMENT_3D('',#28211,#19083,#19084);
#15880=AXIS2_PLACEMENT_3D('',#28236,#19086,#19087);
#15881=AXIS2_PLACEMENT_3D('',#28261,#19089,#19090);
#15882=AXIS2_PLACEMENT_3D('',#28285,#19092,#19093);
#15883=AXIS2_PLACEMENT_3D('',#28309,#19095,#19096);
#15884=AXIS2_PLACEMENT_3D('',#28334,#19098,#19099);
#15885=AXIS2_PLACEMENT_3D('',#28359,#19101,#19102);
#15886=AXIS2_PLACEMENT_3D('',#28383,#19104,#19105);
#15887=AXIS2_PLACEMENT_3D('',#28408,#19107,#19108);
#15888=AXIS2_PLACEMENT_3D('',#28433,#19110,#19111);
#15889=AXIS2_PLACEMENT_3D('',#28457,#19113,#19114);
#15890=AXIS2_PLACEMENT_3D('',#28482,#19116,#19117);
#15891=AXIS2_PLACEMENT_3D('',#28507,#19119,#19120);
#15892=AXIS2_PLACEMENT_3D('',#28531,#19122,#19123);
#15893=AXIS2_PLACEMENT_3D('',#28555,#19125,#19126);
#15894=AXIS2_PLACEMENT_3D('',#28580,#19128,#19129);
#15895=AXIS2_PLACEMENT_3D('',#28605,#19131,#19132);
#15896=AXIS2_PLACEMENT_3D('',#29404,#19134,#19135);
#15897=AXIS2_PLACEMENT_3D('',#29406,#19136,#19137);
#15898=AXIS2_PLACEMENT_3D('',#29407,#19138,#19139);
#15899=AXIS2_PLACEMENT_3D('',#29494,#19140,#19141);
#15900=AXIS2_PLACEMENT_3D('',#29495,#19142,#19143);
#15901=AXIS2_PLACEMENT_3D('',#30181,#19144,#19145);
#15902=AXIS2_PLACEMENT_3D('',#30182,#19146,#19147);
#15903=AXIS2_PLACEMENT_3D('',#30183,#19148,#19149);
#15904=AXIS2_PLACEMENT_3D('',#30185,#19150,#19151);
#15905=AXIS2_PLACEMENT_3D('',#30186,#19152,#19153);
#15906=AXIS2_PLACEMENT_3D('',#30188,#19155,#19156);
#15907=AXIS2_PLACEMENT_3D('',#30212,#19158,#19159);
#15908=AXIS2_PLACEMENT_3D('',#30220,#19160,#19161);
#15909=AXIS2_PLACEMENT_3D('',#30226,#19165,#19166);
#15910=AXIS2_PLACEMENT_3D('',#30230,#19169,#19170);
#15911=AXIS2_PLACEMENT_3D('',#30234,#19173,#19174);
#15912=AXIS2_PLACEMENT_3D('',#30238,#19177,#19178);
#15913=AXIS2_PLACEMENT_3D('',#30242,#19181,#19182);
#15914=AXIS2_PLACEMENT_3D('',#30244,#19184,#19185);
#15915=AXIS2_PLACEMENT_3D('',#30245,#19186,#19187);
#15916=AXIS2_PLACEMENT_3D('',#30246,#19188,#19189);
#15917=AXIS2_PLACEMENT_3D('',#30247,#19190,#19191);
#15918=AXIS2_PLACEMENT_3D('',#30263,#19193,#19194);
#15919=AXIS2_PLACEMENT_3D('',#30271,#19195,#19196);
#15920=AXIS2_PLACEMENT_3D('',#30319,#19198,#19199);
#15921=AXIS2_PLACEMENT_3D('',#30367,#19201,#19202);
#15922=AXIS2_PLACEMENT_3D('',#30421,#19204,#19205);
#15923=AXIS2_PLACEMENT_3D('',#30469,#19207,#19208);
#15924=AXIS2_PLACEMENT_3D('',#30517,#19210,#19211);
#15925=AXIS2_PLACEMENT_3D('',#30565,#19213,#19214);
#15926=AXIS2_PLACEMENT_3D('',#30619,#19216,#19217);
#15927=AXIS2_PLACEMENT_3D('',#30667,#19219,#19220);
#15928=AXIS2_PLACEMENT_3D('',#30715,#19222,#19223);
#15929=AXIS2_PLACEMENT_3D('',#30769,#19225,#19226);
#15930=AXIS2_PLACEMENT_3D('',#30817,#19228,#19229);
#15931=AXIS2_PLACEMENT_3D('',#30865,#19231,#19232);
#15932=AXIS2_PLACEMENT_3D('',#30919,#19234,#19235);
#15933=AXIS2_PLACEMENT_3D('',#30967,#19237,#19238);
#15934=AXIS2_PLACEMENT_3D('',#31015,#19240,#19241);
#15935=AXIS2_PLACEMENT_3D('',#31063,#19243,#19244);
#15936=AXIS2_PLACEMENT_3D('',#31117,#19246,#19247);
#15937=AXIS2_PLACEMENT_3D('',#31165,#19249,#19250);
#15938=AXIS2_PLACEMENT_3D('',#31213,#19252,#19253);
#15939=AXIS2_PLACEMENT_3D('',#31267,#19255,#19256);
#15940=AXIS2_PLACEMENT_3D('',#31315,#19258,#19259);
#15941=AXIS2_PLACEMENT_3D('',#31363,#19261,#19262);
#15942=AXIS2_PLACEMENT_3D('',#31417,#19264,#19265);
#15943=AXIS2_PLACEMENT_3D('',#31465,#19267,#19268);
#15944=AXIS2_PLACEMENT_3D('',#31513,#19270,#19271);
#15945=AXIS2_PLACEMENT_3D('',#31567,#19273,#19274);
#15946=AXIS2_PLACEMENT_3D('',#31615,#19276,#19277);
#15947=AXIS2_PLACEMENT_3D('',#31627,#19279,#19280);
#15948=AXIS2_PLACEMENT_3D('',#31633,#19281,#19282);
#15949=AXIS2_PLACEMENT_3D('',#31657,#19284,#19285);
#15950=AXIS2_PLACEMENT_3D('',#31682,#19287,#19288);
#15951=AXIS2_PLACEMENT_3D('',#31707,#19290,#19291);
#15952=AXIS2_PLACEMENT_3D('',#31731,#19293,#19294);
#15953=AXIS2_PLACEMENT_3D('',#31756,#19296,#19297);
#15954=AXIS2_PLACEMENT_3D('',#31781,#19299,#19300);
#15955=AXIS2_PLACEMENT_3D('',#31805,#19302,#19303);
#15956=AXIS2_PLACEMENT_3D('',#31830,#19305,#19306);
#15957=AXIS2_PLACEMENT_3D('',#31855,#19308,#19309);
#15958=AXIS2_PLACEMENT_3D('',#31879,#19311,#19312);
#15959=AXIS2_PLACEMENT_3D('',#31904,#19314,#19315);
#15960=AXIS2_PLACEMENT_3D('',#31929,#19317,#19318);
#15961=AXIS2_PLACEMENT_3D('',#31953,#19320,#19321);
#15962=AXIS2_PLACEMENT_3D('',#31977,#19323,#19324);
#15963=AXIS2_PLACEMENT_3D('',#32002,#19326,#19327);
#15964=AXIS2_PLACEMENT_3D('',#32027,#19329,#19330);
#15965=AXIS2_PLACEMENT_3D('',#32051,#19332,#19333);
#15966=AXIS2_PLACEMENT_3D('',#32076,#19335,#19336);
#15967=AXIS2_PLACEMENT_3D('',#32101,#19338,#19339);
#15968=AXIS2_PLACEMENT_3D('',#32125,#19341,#19342);
#15969=AXIS2_PLACEMENT_3D('',#32150,#19344,#19345);
#15970=AXIS2_PLACEMENT_3D('',#32175,#19347,#19348);
#15971=AXIS2_PLACEMENT_3D('',#32199,#19350,#19351);
#15972=AXIS2_PLACEMENT_3D('',#32223,#19353,#19354);
#15973=AXIS2_PLACEMENT_3D('',#32248,#19356,#19357);
#15974=AXIS2_PLACEMENT_3D('',#32273,#19359,#19360);
#15975=AXIS2_PLACEMENT_3D('',#33228,#19362,#19363);
#15976=AXIS2_PLACEMENT_3D('',#33230,#19364,#19365);
#15977=AXIS2_PLACEMENT_3D('',#33231,#19366,#19367);
#15978=AXIS2_PLACEMENT_3D('',#33318,#19368,#19369);
#15979=AXIS2_PLACEMENT_3D('',#33319,#19370,#19371);
#15980=AXIS2_PLACEMENT_3D('',#34161,#19372,#19373);
#15981=AXIS2_PLACEMENT_3D('',#34165,#19375,#19376);
#15982=AXIS2_PLACEMENT_3D('',#34166,#19377,#19378);
#15983=AXIS2_PLACEMENT_3D('',#34180,#19382,#19383);
#15984=AXIS2_PLACEMENT_3D('',#34191,#19386,#19387);
#15985=AXIS2_PLACEMENT_3D('',#34202,#19390,#19391);
#15986=AXIS2_PLACEMENT_3D('',#34213,#19394,#19395);
#15987=AXIS2_PLACEMENT_3D('',#34224,#19398,#19399);
#15988=AXIS2_PLACEMENT_3D('',#34232,#19401,#19402);
#15989=AXIS2_PLACEMENT_3D('',#34233,#19403,#19404);
#15990=AXIS2_PLACEMENT_3D('',#34235,#19405,#19406);
#15991=AXIS2_PLACEMENT_3D('',#34236,#19407,#19408);
#15992=AXIS2_PLACEMENT_3D('',#34238,#19410,#19411);
#15993=AXIS2_PLACEMENT_3D('',#34239,#19412,#19413);
#15994=AXIS2_PLACEMENT_3D('',#34240,#19414,#19415);
#15995=AXIS2_PLACEMENT_3D('',#34242,#19416,#19417);
#15996=AXIS2_PLACEMENT_3D('',#34243,#19418,#19419);
#15997=AXIS2_PLACEMENT_3D('',#34246,#19420,#19421);
#15998=AXIS2_PLACEMENT_3D('',#34248,#19423,#19424);
#15999=AXIS2_PLACEMENT_3D('',#34279,#19425,#19426);
#16000=AXIS2_PLACEMENT_3D('',#34280,#19427,#19428);
#16001=AXIS2_PLACEMENT_3D('',#34282,#19429,#19430);
#16002=AXIS2_PLACEMENT_3D('',#34286,#19432,#19433);
#16003=AXIS2_PLACEMENT_3D('',#34287,#19434,#19435);
#16004=AXIS2_PLACEMENT_3D('',#34288,#19436,#19437);
#16005=AXIS2_PLACEMENT_3D('',#34291,#19439,#19440);
#16006=AXIS2_PLACEMENT_3D('',#34292,#19441,#19442);
#16007=AXIS2_PLACEMENT_3D('',#34294,#19443,#19444);
#16008=AXIS2_PLACEMENT_3D('',#34295,#19445,#19446);
#16009=AXIS2_PLACEMENT_3D('',#34298,#19448,#19449);
#16010=AXIS2_PLACEMENT_3D('',#34299,#19450,#19451);
#16011=AXIS2_PLACEMENT_3D('',#34301,#19452,#19453);
#16012=AXIS2_PLACEMENT_3D('',#34302,#19454,#19455);
#16013=AXIS2_PLACEMENT_3D('',#34304,#19457,#19458);
#16014=AXIS2_PLACEMENT_3D('',#34305,#19459,#19460);
#16015=AXIS2_PLACEMENT_3D('',#34318,#19463,#19464);
#16016=AXIS2_PLACEMENT_3D('',#34328,#19466,#19467);
#16017=AXIS2_PLACEMENT_3D('',#34351,#19469,#19470);
#16018=AXIS2_PLACEMENT_3D('',#34375,#19471,#19472);
#16019=AXIS2_PLACEMENT_3D('',#34377,#19473,#19474);
#16020=AXIS2_PLACEMENT_3D('',#34380,#19476,#19477);
#16021=AXIS2_PLACEMENT_3D('',#34381,#19478,#19479);
#16022=AXIS2_PLACEMENT_3D('',#34384,#19481,#19482);
#16023=AXIS2_PLACEMENT_3D('',#34385,#19483,#19484);
#16024=AXIS2_PLACEMENT_3D('',#34387,#19485,#19486);
#16025=AXIS2_PLACEMENT_3D('',#34388,#19487,#19488);
#16026=AXIS2_PLACEMENT_3D('',#34390,#19489,#19490);
#16027=AXIS2_PLACEMENT_3D('',#34392,#19492,#19493);
#16028=AXIS2_PLACEMENT_3D('',#34393,#19494,#19495);
#16029=AXIS2_PLACEMENT_3D('',#34401,#19498,#19499);
#16030=AXIS2_PLACEMENT_3D('',#34407,#19501,#19502);
#16031=AXIS2_PLACEMENT_3D('',#34443,#19504,#19505);
#16032=AXIS2_PLACEMENT_3D('',#34445,#19507,#19508);
#16033=AXIS2_PLACEMENT_3D('',#34447,#19510,#19511);
#16034=AXIS2_PLACEMENT_3D('',#34449,#19513,#19514);
#16035=AXIS2_PLACEMENT_3D('',#34451,#19516,#19517);
#16036=AXIS2_PLACEMENT_3D('',#34453,#19519,#19520);
#16037=AXIS2_PLACEMENT_3D('',#34455,#19522,#19523);
#16038=AXIS2_PLACEMENT_3D('',#34456,#19524,#19525);
#16039=AXIS2_PLACEMENT_3D('',#34457,#19526,#19527);
#16040=AXIS2_PLACEMENT_3D('',#34458,#19528,#19529);
#16041=AXIS2_PLACEMENT_3D('',#34474,#19531,#19532);
#16042=AXIS2_PLACEMENT_3D('',#34482,#19533,#19534);
#16043=AXIS2_PLACEMENT_3D('',#34530,#19536,#19537);
#16044=AXIS2_PLACEMENT_3D('',#34578,#19539,#19540);
#16045=AXIS2_PLACEMENT_3D('',#34629,#19542,#19543);
#16046=AXIS2_PLACEMENT_3D('',#34680,#19545,#19546);
#16047=AXIS2_PLACEMENT_3D('',#34728,#19548,#19549);
#16048=AXIS2_PLACEMENT_3D('',#34776,#19551,#19552);
#16049=AXIS2_PLACEMENT_3D('',#34830,#19554,#19555);
#16050=AXIS2_PLACEMENT_3D('',#34878,#19557,#19558);
#16051=AXIS2_PLACEMENT_3D('',#34926,#19560,#19561);
#16052=AXIS2_PLACEMENT_3D('',#34980,#19563,#19564);
#16053=AXIS2_PLACEMENT_3D('',#35028,#19566,#19567);
#16054=AXIS2_PLACEMENT_3D('',#35076,#19569,#19570);
#16055=AXIS2_PLACEMENT_3D('',#35124,#19572,#19573);
#16056=AXIS2_PLACEMENT_3D('',#35178,#19575,#19576);
#16057=AXIS2_PLACEMENT_3D('',#35226,#19578,#19579);
#16058=AXIS2_PLACEMENT_3D('',#35274,#19581,#19582);
#16059=AXIS2_PLACEMENT_3D('',#35279,#19584,#19585);
#16060=AXIS2_PLACEMENT_3D('',#35327,#19586,#19587);
#16061=AXIS2_PLACEMENT_3D('',#35341,#19589,#19590);
#16062=AXIS2_PLACEMENT_3D('',#35348,#19591,#19592);
#16063=AXIS2_PLACEMENT_3D('',#35373,#19594,#19595);
#16064=AXIS2_PLACEMENT_3D('',#35397,#19597,#19598);
#16065=AXIS2_PLACEMENT_3D('',#35422,#19600,#19601);
#16066=AXIS2_PLACEMENT_3D('',#35447,#19603,#19604);
#16067=AXIS2_PLACEMENT_3D('',#35471,#19606,#19607);
#16068=AXIS2_PLACEMENT_3D('',#35495,#19609,#19610);
#16069=AXIS2_PLACEMENT_3D('',#35520,#19612,#19613);
#16070=AXIS2_PLACEMENT_3D('',#35545,#19615,#19616);
#16071=AXIS2_PLACEMENT_3D('',#35569,#19618,#19619);
#16072=AXIS2_PLACEMENT_3D('',#35594,#19621,#19622);
#16073=AXIS2_PLACEMENT_3D('',#35619,#19624,#19625);
#16074=AXIS2_PLACEMENT_3D('',#35643,#19627,#19628);
#16075=AXIS2_PLACEMENT_3D('',#35668,#19630,#19631);
#16076=AXIS2_PLACEMENT_3D('',#35692,#19633,#19634);
#16077=AXIS2_PLACEMENT_3D('',#35717,#19636,#19637);
#16078=AXIS2_PLACEMENT_3D('',#36376,#19639,#19640);
#16079=AXIS2_PLACEMENT_3D('',#36378,#19641,#19642);
#16080=AXIS2_PLACEMENT_3D('',#36379,#19643,#19644);
#16081=AXIS2_PLACEMENT_3D('',#36463,#19645,#19646);
#16082=AXIS2_PLACEMENT_3D('',#36464,#19647,#19648);
#16083=AXIS2_PLACEMENT_3D('',#37011,#19649,#19650);
#16084=AXIS2_PLACEMENT_3D('',#37015,#19652,#19653);
#16085=AXIS2_PLACEMENT_3D('',#37016,#19654,#19655);
#16086=AXIS2_PLACEMENT_3D('',#37030,#19659,#19660);
#16087=AXIS2_PLACEMENT_3D('',#37041,#19663,#19664);
#16088=AXIS2_PLACEMENT_3D('',#37052,#19667,#19668);
#16089=AXIS2_PLACEMENT_3D('',#37063,#19671,#19672);
#16090=AXIS2_PLACEMENT_3D('',#37074,#19675,#19676);
#16091=AXIS2_PLACEMENT_3D('',#37082,#19678,#19679);
#16092=AXIS2_PLACEMENT_3D('',#37083,#19680,#19681);
#16093=AXIS2_PLACEMENT_3D('',#37085,#19682,#19683);
#16094=AXIS2_PLACEMENT_3D('',#37086,#19684,#19685);
#16095=AXIS2_PLACEMENT_3D('',#37088,#19687,#19688);
#16096=AXIS2_PLACEMENT_3D('',#37089,#19689,#19690);
#16097=AXIS2_PLACEMENT_3D('',#37090,#19691,#19692);
#16098=AXIS2_PLACEMENT_3D('',#37092,#19693,#19694);
#16099=AXIS2_PLACEMENT_3D('',#37093,#19695,#19696);
#16100=AXIS2_PLACEMENT_3D('',#37096,#19697,#19698);
#16101=AXIS2_PLACEMENT_3D('',#37098,#19700,#19701);
#16102=AXIS2_PLACEMENT_3D('',#37129,#19702,#19703);
#16103=AXIS2_PLACEMENT_3D('',#37130,#19704,#19705);
#16104=AXIS2_PLACEMENT_3D('',#37131,#19706,#19707);
#16105=AXIS2_PLACEMENT_3D('',#37132,#19708,#19709);
#16106=AXIS2_PLACEMENT_3D('',#37133,#19710,#19711);
#16107=AXIS2_PLACEMENT_3D('',#37134,#19712,#19713);
#16108=AXIS2_PLACEMENT_3D('',#37135,#19714,#19715);
#16109=AXIS2_PLACEMENT_3D('',#37136,#19716,#19717);
#16110=AXIS2_PLACEMENT_3D('',#37137,#19718,#19719);
#16111=AXIS2_PLACEMENT_3D('',#37138,#19720,#19721);
#16112=AXIS2_PLACEMENT_3D('',#37139,#19722,#19723);
#16113=AXIS2_PLACEMENT_3D('',#37140,#19724,#19725);
#16114=AXIS2_PLACEMENT_3D('',#37141,#19726,#19727);
#16115=AXIS2_PLACEMENT_3D('',#37142,#19728,#19729);
#16116=AXIS2_PLACEMENT_3D('',#37143,#19730,#19731);
#16117=AXIS2_PLACEMENT_3D('',#37144,#19732,#19733);
#16118=AXIS2_PLACEMENT_3D('',#37145,#19734,#19735);
#16119=AXIS2_PLACEMENT_3D('',#37146,#19736,#19737);
#16120=AXIS2_PLACEMENT_3D('',#37147,#19738,#19739);
#16121=AXIS2_PLACEMENT_3D('',#37148,#19740,#19741);
#16122=AXIS2_PLACEMENT_3D('',#37149,#19742,#19743);
#16123=AXIS2_PLACEMENT_3D('',#37150,#19744,#19745);
#16124=AXIS2_PLACEMENT_3D('',#37151,#19746,#19747);
#16125=DIRECTION('axis',(0.,0.,1.));
#16126=DIRECTION('refdir',(1.,0.,0.));
#16127=DIRECTION('axis',(0.,0.,1.));
#16128=DIRECTION('refdir',(1.,0.,0.));
#16129=DIRECTION('center_axis',(-0.693904010166723,0.,-0.720067513969725));
#16130=DIRECTION('ref_axis',(-0.720067513969725,0.,0.693904010166723));
#16131=DIRECTION('',(0.591591578932266,-0.570096221587387,-0.570096221587386));
#16132=DIRECTION('',(0.,-1.,0.));
#16133=DIRECTION('',(-0.591591578932266,-0.570096221587387,0.570096221587386));
#16134=DIRECTION('',(0.,1.,0.));
#16135=DIRECTION('center_axis',(0.,0.707106781186547,-0.707106781186548));
#16136=DIRECTION('ref_axis',(-1.,0.,0.));
#16137=DIRECTION('',(1.,0.,0.));
#16138=DIRECTION('',(0.,-0.707106781186548,-0.707106781186547));
#16139=DIRECTION('',(-1.,0.,0.));
#16140=DIRECTION('center_axis',(0.,1.,0.));
#16141=DIRECTION('ref_axis',(1.,0.,0.));
#16142=DIRECTION('center_axis',(0.,-1.,0.));
#16143=DIRECTION('ref_axis',(1.,0.,0.));
#16144=DIRECTION('center_axis',(0.,1.,0.));
#16145=DIRECTION('ref_axis',(1.,0.,0.));
#16146=DIRECTION('center_axis',(0.,1.,0.));
#16147=DIRECTION('ref_axis',(1.,0.,0.));
#16148=DIRECTION('center_axis',(0.,1.,0.));
#16149=DIRECTION('ref_axis',(1.,0.,0.));
#16150=DIRECTION('',(0.,-1.,0.));
#16151=DIRECTION('center_axis',(0.577350269189625,0.577350269189626,-0.577350269189626));
#16152=DIRECTION('ref_axis',(-0.707106781186548,0.,-0.707106781186547));
#16153=DIRECTION('',(-0.707106781186547,0.707106781186547,4.08878244448899E-16));
#16154=DIRECTION('',(0.707106781186548,0.,0.707106781186547));
#16155=DIRECTION('center_axis',(0.577350269189625,-0.577350269189626,-0.577350269189626));
#16156=DIRECTION('ref_axis',(-0.707106781186548,0.,-0.707106781186547));
#16157=DIRECTION('',(-0.707106781186548,0.,-0.707106781186547));
#16158=DIRECTION('',(0.707106781186547,0.707106781186547,-4.08878244448899E-16));
#16159=DIRECTION('',(0.,-0.707106781186548,0.707106781186547));
#16160=DIRECTION('center_axis',(0.707106781186548,-0.707106781186548,0.));
#16161=DIRECTION('ref_axis',(0.,0.,-1.));
#16162=DIRECTION('',(-0.707106781186547,-0.707106781186547,0.));
#16163=DIRECTION('',(0.,0.,-1.));
#16164=DIRECTION('',(0.,0.,1.));
#16165=DIRECTION('center_axis',(0.,1.,0.));
#16166=DIRECTION('ref_axis',(0.707106781186549,0.,0.707106781186546));
#16167=DIRECTION('center_axis',(0.,-1.,0.));
#16168=DIRECTION('ref_axis',(0.707106781186549,0.,0.707106781186546));
#16169=DIRECTION('',(0.,-0.707106781186547,-0.707106781186548));
#16170=DIRECTION('center_axis',(0.,1.,0.));
#16171=DIRECTION('ref_axis',(0.707106781186549,0.,0.707106781186546));
#16172=DIRECTION('center_axis',(0.,-0.707106781186548,0.707106781186548));
#16173=DIRECTION('ref_axis',(1.,0.,0.));
#16174=DIRECTION('',(1.,0.,0.));
#16175=DIRECTION('',(-1.,0.,0.));
#16176=DIRECTION('center_axis',(0.,-0.707106781186547,-0.707106781186548));
#16177=DIRECTION('ref_axis',(-1.,0.,0.));
#16178=DIRECTION('',(1.,0.,0.));
#16179=DIRECTION('',(-1.,0.,0.));
#16180=DIRECTION('center_axis',(0.707106781186547,0.,-0.707106781186548));
#16181=DIRECTION('ref_axis',(-0.707106781186548,0.,-0.707106781186547));
#16182=DIRECTION('',(0.,-1.,0.));
#16183=DIRECTION('',(0.,1.,0.));
#16184=DIRECTION('center_axis',(0.,0.707106781186548,0.707106781186548));
#16185=DIRECTION('ref_axis',(1.,0.,0.));
#16186=DIRECTION('',(1.,0.,0.));
#16187=DIRECTION('',(0.,0.707106781186547,-0.707106781186547));
#16188=DIRECTION('',(-1.,0.,0.));
#16189=DIRECTION('center_axis',(0.,-1.,0.));
#16190=DIRECTION('ref_axis',(0.707106781186549,0.,0.707106781186546));
#16191=DIRECTION('center_axis',(0.,1.,0.));
#16192=DIRECTION('ref_axis',(0.707106781186549,0.,0.707106781186546));
#16193=DIRECTION('',(-0.707106781186547,0.707106781186547,-8.17756488897799E-16));
#16194=DIRECTION('center_axis',(0.,-1.,0.));
#16195=DIRECTION('ref_axis',(0.707106781186549,0.,0.707106781186546));
#16196=DIRECTION('center_axis',(0.707106781186548,0.707106781186548,0.));
#16197=DIRECTION('ref_axis',(0.,0.,-1.));
#16198=DIRECTION('',(0.,0.,-1.));
#16199=DIRECTION('',(0.,0.,1.));
#16200=DIRECTION('center_axis',(0.,1.,0.));
#16201=DIRECTION('ref_axis',(1.,0.,0.));
#16202=DIRECTION('center_axis',(0.,1.,0.));
#16203=DIRECTION('ref_axis',(1.,0.,0.));
#16204=DIRECTION('',(1.,0.,0.));
#16205=DIRECTION('center_axis',(0.,1.,0.));
#16206=DIRECTION('ref_axis',(-0.707106781186546,0.,0.707106781186549));
#16207=DIRECTION('',(0.,0.,1.));
#16208=DIRECTION('',(-1.,0.,0.));
#16209=DIRECTION('center_axis',(0.,-1.,0.));
#16210=DIRECTION('ref_axis',(1.,0.,0.));
#16211=DIRECTION('center_axis',(1.,0.,0.));
#16212=DIRECTION('ref_axis',(0.,0.,-1.));
#16213=DIRECTION('',(0.,1.,0.));
#16214=DIRECTION('center_axis',(0.,1.,0.));
#16215=DIRECTION('ref_axis',(0.707106781186549,0.,0.707106781186546));
#16216=DIRECTION('',(0.,-1.,0.));
#16217=DIRECTION('center_axis',(0.,0.,1.));
#16218=DIRECTION('ref_axis',(1.,0.,0.));
#16219=DIRECTION('',(0.,1.,0.));
#16220=DIRECTION('center_axis',(0.,0.,-1.));
#16221=DIRECTION('ref_axis',(1.,0.,0.));
#16222=DIRECTION('center_axis',(0.693904010166723,0.,-0.720067513969725));
#16223=DIRECTION('ref_axis',(-0.720067513969725,0.,-0.693904010166723));
#16224=DIRECTION('',(-0.591591578932266,0.570096221587387,-0.570096221587386));
#16225=DIRECTION('',(0.,1.,0.));
#16226=DIRECTION('',(0.591591578932266,0.570096221587387,0.570096221587386));
#16227=DIRECTION('center_axis',(0.,0.707106781186547,-0.707106781186548));
#16228=DIRECTION('ref_axis',(-1.,0.,0.));
#16229=DIRECTION('',(-1.,0.,0.));
#16230=DIRECTION('',(0.,0.707106781186548,0.707106781186547));
#16231=DIRECTION('',(1.,0.,0.));
#16232=DIRECTION('center_axis',(-0.577350269189626,0.577350269189626,-0.577350269189626));
#16233=DIRECTION('ref_axis',(-0.707106781186548,0.,0.707106781186547));
#16234=DIRECTION('',(0.707106781186548,0.,-0.707106781186547));
#16235=DIRECTION('',(-0.707106781186547,-0.707106781186547,4.08878244448899E-16));
#16236=DIRECTION('center_axis',(-0.577350269189626,-0.577350269189626,-0.577350269189626));
#16237=DIRECTION('ref_axis',(-0.707106781186548,0.,0.707106781186547));
#16238=DIRECTION('',(-0.707106781186548,0.,0.707106781186547));
#16239=DIRECTION('',(0.,0.707106781186548,-0.707106781186547));
#16240=DIRECTION('',(0.707106781186547,-0.707106781186547,-4.08878244448899E-16));
#16241=DIRECTION('center_axis',(0.,-0.707106781186547,-0.707106781186548));
#16242=DIRECTION('ref_axis',(-1.,0.,0.));
#16243=DIRECTION('',(1.,0.,0.));
#16244=DIRECTION('center_axis',(0.,-0.707106781186548,0.707106781186548));
#16245=DIRECTION('ref_axis',(1.,0.,0.));
#16246=DIRECTION('',(-1.,0.,0.));
#16247=DIRECTION('',(0.,-0.707106781186547,-0.707106781186547));
#16248=DIRECTION('center_axis',(0.,1.,0.));
#16249=DIRECTION('ref_axis',(-0.707106781186546,0.,0.707106781186549));
#16250=DIRECTION('center_axis',(0.,-1.,0.));
#16251=DIRECTION('ref_axis',(-0.707106781186546,0.,0.707106781186549));
#16252=DIRECTION('',(0.707106781186541,-0.707106781186554,0.));
#16253=DIRECTION('center_axis',(-0.707106781186548,-0.707106781186548,0.));
#16254=DIRECTION('ref_axis',(0.,0.,1.));
#16255=DIRECTION('',(0.,0.,-1.));
#16256=DIRECTION('center_axis',(-0.707106781186547,0.,-0.707106781186548));
#16257=DIRECTION('ref_axis',(-0.707106781186548,0.,0.707106781186547));
#16258=DIRECTION('',(0.,-1.,0.));
#16259=DIRECTION('',(0.,1.,0.));
#16260=DIRECTION('center_axis',(-0.707106781186548,0.707106781186548,0.));
#16261=DIRECTION('ref_axis',(0.,0.,1.));
#16262=DIRECTION('',(0.707106781186547,0.707106781186547,0.));
#16263=DIRECTION('',(0.,0.,-1.));
#16264=DIRECTION('',(0.,0.,1.));
#16265=DIRECTION('center_axis',(0.,-1.,0.));
#16266=DIRECTION('ref_axis',(-0.707106781186546,0.,0.707106781186549));
#16267=DIRECTION('center_axis',(0.,1.,0.));
#16268=DIRECTION('ref_axis',(-0.707106781186546,0.,0.707106781186549));
#16269=DIRECTION('',(0.,0.707106781186545,-0.70710678118655));
#16270=DIRECTION('center_axis',(0.,-1.,0.));
#16271=DIRECTION('ref_axis',(-0.707106781186546,0.,0.707106781186549));
#16272=DIRECTION('center_axis',(0.,0.707106781186548,0.707106781186548));
#16273=DIRECTION('ref_axis',(1.,0.,0.));
#16274=DIRECTION('',(-1.,0.,0.));
#16275=DIRECTION('',(1.,0.,0.));
#16276=DIRECTION('center_axis',(0.,-1.,0.));
#16277=DIRECTION('ref_axis',(1.,0.,0.));
#16278=DIRECTION('center_axis',(0.,0.,-1.));
#16279=DIRECTION('ref_axis',(-1.,0.,0.));
#16280=DIRECTION('center_axis',(0.,0.,1.));
#16281=DIRECTION('ref_axis',(1.,0.,0.));
#16282=DIRECTION('center_axis',(0.,1.,0.));
#16283=DIRECTION('ref_axis',(1.,0.,0.));
#16284=DIRECTION('center_axis',(0.,-1.,0.));
#16285=DIRECTION('ref_axis',(1.,0.,0.));
#16286=DIRECTION('center_axis',(0.,-1.,0.));
#16287=DIRECTION('ref_axis',(1.,0.,0.));
#16288=DIRECTION('center_axis',(0.,1.,0.));
#16289=DIRECTION('ref_axis',(1.,0.,0.));
#16290=DIRECTION('center_axis',(0.,-1.,0.));
#16291=DIRECTION('ref_axis',(1.,0.,0.));
#16292=DIRECTION('center_axis',(0.,1.,0.));
#16293=DIRECTION('ref_axis',(1.,0.,0.));
#16294=DIRECTION('',(0.,1.,0.));
#16295=DIRECTION('center_axis',(0.,0.,-1.));
#16296=DIRECTION('ref_axis',(1.,0.,0.));
#16297=DIRECTION('',(0.,0.,-1.));
#16298=DIRECTION('center_axis',(0.,0.,1.));
#16299=DIRECTION('ref_axis',(1.,0.,0.));
#16300=DIRECTION('center_axis',(0.,0.,-1.));
#16301=DIRECTION('ref_axis',(1.,0.,0.));
#16302=DIRECTION('center_axis',(0.,0.,-1.));
#16303=DIRECTION('ref_axis',(1.,0.,0.));
#16304=DIRECTION('',(0.,0.,-1.));
#16305=DIRECTION('center_axis',(0.,1.,0.));
#16306=DIRECTION('ref_axis',(1.,0.,0.));
#16307=DIRECTION('center_axis',(0.,1.,0.));
#16308=DIRECTION('ref_axis',(-0.707106781186546,0.,0.707106781186549));
#16309=DIRECTION('',(0.,1.,0.));
#16310=DIRECTION('',(0.,-1.,0.));
#16311=DIRECTION('center_axis',(0.,0.,1.));
#16312=DIRECTION('ref_axis',(1.,0.,0.));
#16313=DIRECTION('center_axis',(-1.,0.,0.));
#16314=DIRECTION('ref_axis',(0.,0.,1.));
#16315=DIRECTION('center_axis',(0.,0.,-1.));
#16316=DIRECTION('ref_axis',(-1.,0.,0.));
#16317=DIRECTION('axis',(0.,0.,1.));
#16318=DIRECTION('refdir',(1.,0.,0.));
#16319=DIRECTION('center_axis',(0.707106781186548,-0.707106781186548,0.));
#16320=DIRECTION('ref_axis',(0.,0.,-1.));
#16321=DIRECTION('',(0.577350269189626,0.577350269189626,-0.577350269189626));
#16322=DIRECTION('',(0.,0.,-1.));
#16323=DIRECTION('',(0.707106781186547,0.707106781186547,0.));
#16324=DIRECTION('',(0.,0.,1.));
#16325=DIRECTION('center_axis',(-1.,0.,0.));
#16326=DIRECTION('ref_axis',(0.,-0.707106781186547,-0.707106781186548));
#16327=DIRECTION('center_axis',(1.,0.,0.));
#16328=DIRECTION('ref_axis',(0.,-0.707106781186547,-0.707106781186548));
#16329=DIRECTION('',(0.707106781186551,4.08878244448901E-16,0.707106781186544));
#16330=DIRECTION('center_axis',(-1.,0.,0.));
#16331=DIRECTION('ref_axis',(0.,-0.707106781186547,-0.707106781186548));
#16332=DIRECTION('center_axis',(0.707106781186548,0.,-0.707106781186548));
#16333=DIRECTION('ref_axis',(-0.707106781186548,0.,-0.707106781186548));
#16334=DIRECTION('',(0.707106781186547,0.,0.707106781186547));
#16335=DIRECTION('',(0.,-1.,0.));
#16336=DIRECTION('',(0.,1.,0.));
#16337=DIRECTION('center_axis',(-1.,0.,0.));
#16338=DIRECTION('ref_axis',(0.,0.707106781186547,-0.707106781186548));
#16339=DIRECTION('center_axis',(1.,0.,0.));
#16340=DIRECTION('ref_axis',(0.,0.707106781186547,-0.707106781186548));
#16341=DIRECTION('',(0.707106781186549,-0.707106781186546,0.));
#16342=DIRECTION('center_axis',(-1.,0.,0.));
#16343=DIRECTION('ref_axis',(0.,0.707106781186547,-0.707106781186548));
#16344=DIRECTION('center_axis',(0.707106781186548,0.707106781186548,0.));
#16345=DIRECTION('ref_axis',(0.,0.,-1.));
#16346=DIRECTION('',(0.,0.,-1.));
#16347=DIRECTION('',(0.,0.,1.));
#16348=DIRECTION('',(0.577350269189626,-0.577350269189626,-0.577350269189626));
#16349=DIRECTION('center_axis',(0.,0.707106781186548,-0.707106781186548));
#16350=DIRECTION('ref_axis',(-1.,0.,0.));
#16351=DIRECTION('',(1.,0.,0.));
#16352=DIRECTION('',(-1.,0.,0.));
#16353=DIRECTION('center_axis',(1.,0.,0.));
#16354=DIRECTION('ref_axis',(0.,0.,-1.));
#16355=DIRECTION('',(0.,1.,0.));
#16356=DIRECTION('center_axis',(-1.,0.,0.));
#16357=DIRECTION('ref_axis',(0.,0.,-1.));
#16358=DIRECTION('center_axis',(0.,0.,-1.));
#16359=DIRECTION('ref_axis',(-1.,0.,0.));
#16360=DIRECTION('',(0.,1.,0.));
#16361=DIRECTION('',(1.,0.,0.));
#16362=DIRECTION('center_axis',(0.,0.707106781186548,-0.707106781186548));
#16363=DIRECTION('ref_axis',(-1.,0.,0.));
#16364=DIRECTION('',(-1.,0.,0.));
#16365=DIRECTION('',(0.,0.707106781186547,0.707106781186547));
#16366=DIRECTION('',(1.,0.,0.));
#16367=DIRECTION('',(-0.577350269189626,-0.577350269189626,-0.577350269189626));
#16368=DIRECTION('center_axis',(-0.707106781186548,-0.707106781186548,0.));
#16369=DIRECTION('ref_axis',(0.,0.,1.));
#16370=DIRECTION('',(0.,0.,-1.));
#16371=DIRECTION('',(0.707106781186547,-0.707106781186547,0.));
#16372=DIRECTION('',(0.,0.,1.));
#16373=DIRECTION('',(-0.577350269189625,0.577350269189625,-0.577350269189627));
#16374=DIRECTION('center_axis',(0.,-0.707106781186548,-0.707106781186548));
#16375=DIRECTION('ref_axis',(-1.,0.,0.));
#16376=DIRECTION('',(-1.,0.,0.));
#16377=DIRECTION('',(0.,0.707106781186547,-0.707106781186547));
#16378=DIRECTION('',(1.,0.,0.));
#16379=DIRECTION('center_axis',(0.,1.,0.));
#16380=DIRECTION('ref_axis',(-0.707106781186549,0.,-0.707106781186546));
#16381=DIRECTION('',(-0.707106781186547,0.707106781186547,-8.17756488897799E-16));
#16382=DIRECTION('center_axis',(0.,-1.,0.));
#16383=DIRECTION('ref_axis',(-0.707106781186549,0.,-0.707106781186546));
#16384=DIRECTION('center_axis',(0.,1.,0.));
#16385=DIRECTION('ref_axis',(-0.707106781186549,0.,-0.707106781186546));
#16386=DIRECTION('center_axis',(-0.707106781186548,-0.707106781186548,0.));
#16387=DIRECTION('ref_axis',(0.,0.,1.));
#16388=DIRECTION('',(-0.577350269189626,0.577350269189626,-0.577350269189626));
#16389=DIRECTION('',(0.,0.,-1.));
#16390=DIRECTION('',(0.,0.,1.));
#16391=DIRECTION('',(-0.577350269189626,0.577350269189626,0.577350269189625));
#16392=DIRECTION('center_axis',(1.,0.,0.));
#16393=DIRECTION('ref_axis',(0.,-0.707106781186547,-0.707106781186548));
#16394=DIRECTION('',(0.707106781186551,-4.08878244448901E-16,-0.707106781186544));
#16395=DIRECTION('center_axis',(-1.,0.,0.));
#16396=DIRECTION('ref_axis',(0.,-0.707106781186547,-0.707106781186548));
#16397=DIRECTION('center_axis',(1.,0.,0.));
#16398=DIRECTION('ref_axis',(0.,-0.707106781186547,-0.707106781186548));
#16399=DIRECTION('center_axis',(-0.707106781186548,0.,-0.707106781186548));
#16400=DIRECTION('ref_axis',(-0.707106781186548,0.,0.707106781186548));
#16401=DIRECTION('',(0.707106781186547,0.,-0.707106781186547));
#16402=DIRECTION('',(0.,-1.,0.));
#16403=DIRECTION('',(0.,1.,0.));
#16404=DIRECTION('center_axis',(1.,0.,0.));
#16405=DIRECTION('ref_axis',(0.,0.707106781186547,-0.707106781186548));
#16406=DIRECTION('',(0.707106781186549,0.707106781186546,0.));
#16407=DIRECTION('center_axis',(-1.,0.,0.));
#16408=DIRECTION('ref_axis',(0.,0.707106781186547,-0.707106781186548));
#16409=DIRECTION('center_axis',(1.,0.,0.));
#16410=DIRECTION('ref_axis',(0.,0.707106781186547,-0.707106781186548));
#16411=DIRECTION('center_axis',(-0.707106781186548,0.707106781186548,0.));
#16412=DIRECTION('ref_axis',(0.,0.,1.));
#16413=DIRECTION('',(0.,0.,-1.));
#16414=DIRECTION('',(0.,0.,1.));
#16415=DIRECTION('center_axis',(0.,-1.,0.));
#16416=DIRECTION('ref_axis',(-0.707106781186549,0.,-0.707106781186546));
#16417=DIRECTION('center_axis',(0.,1.,0.));
#16418=DIRECTION('ref_axis',(-0.707106781186549,0.,-0.707106781186546));
#16419=DIRECTION('',(0.707106781186547,0.707106781186547,8.17756488897799E-16));
#16420=DIRECTION('center_axis',(0.,-1.,0.));
#16421=DIRECTION('ref_axis',(-0.707106781186549,0.,-0.707106781186546));
#16422=DIRECTION('center_axis',(-0.707106781186548,0.707106781186548,0.));
#16423=DIRECTION('ref_axis',(0.,0.,1.));
#16424=DIRECTION('',(0.577350269189626,0.577350269189626,-0.577350269189625));
#16425=DIRECTION('',(0.,0.,-1.));
#16426=DIRECTION('',(0.,0.,1.));
#16427=DIRECTION('',(0.577350269189626,0.577350269189626,0.577350269189626));
#16428=DIRECTION('center_axis',(0.,1.,0.));
#16429=DIRECTION('ref_axis',(1.,0.,0.));
#16430=DIRECTION('',(-1.,0.,0.));
#16431=DIRECTION('center_axis',(0.,1.,0.));
#16432=DIRECTION('ref_axis',(1.,0.,0.));
#16433=DIRECTION('',(-1.,0.,0.));
#16434=DIRECTION('',(0.,0.,1.));
#16435=DIRECTION('',(-1.,0.,0.));
#16436=DIRECTION('',(0.,0.,-1.));
#16437=DIRECTION('',(-1.,0.,0.));
#16438=DIRECTION('center_axis',(0.,1.,0.));
#16439=DIRECTION('ref_axis',(0.707106781186546,0.,-0.707106781186549));
#16440=DIRECTION('',(0.,0.,-1.));
#16441=DIRECTION('',(1.,0.,0.));
#16442=DIRECTION('center_axis',(0.,-1.,0.));
#16443=DIRECTION('ref_axis',(1.,0.,0.));
#16444=DIRECTION('',(1.,0.,0.));
#16445=DIRECTION('',(-1.,0.,0.));
#16446=DIRECTION('center_axis',(-1.,0.,0.));
#16447=DIRECTION('ref_axis',(0.,-0.707106781186547,-0.707106781186548));
#16448=DIRECTION('',(1.,0.,0.));
#16449=DIRECTION('center_axis',(0.,0.,-1.));
#16450=DIRECTION('ref_axis',(-1.,0.,0.));
#16451=DIRECTION('',(-1.,0.,0.));
#16452=DIRECTION('center_axis',(-1.,0.,0.));
#16453=DIRECTION('ref_axis',(0.,0.707106781186547,-0.707106781186548));
#16454=DIRECTION('',(1.,0.,0.));
#16455=DIRECTION('center_axis',(0.,1.,0.));
#16456=DIRECTION('ref_axis',(1.,0.,0.));
#16457=DIRECTION('',(-1.,0.,0.));
#16458=DIRECTION('center_axis',(0.,1.,0.));
#16459=DIRECTION('ref_axis',(1.,0.,0.));
#16460=DIRECTION('',(-1.,0.,0.));
#16461=DIRECTION('',(0.,0.,1.));
#16462=DIRECTION('center_axis',(0.,-1.,0.));
#16463=DIRECTION('ref_axis',(0.707106781186546,0.,-0.707106781186549));
#16464=DIRECTION('',(1.,0.,0.));
#16465=DIRECTION('',(0.,0.,1.));
#16466=DIRECTION('',(1.,0.,0.));
#16467=DIRECTION('',(0.,0.,-1.));
#16468=DIRECTION('',(1.,0.,0.));
#16469=DIRECTION('center_axis',(0.,-1.,0.));
#16470=DIRECTION('ref_axis',(1.,0.,0.));
#16471=DIRECTION('center_axis',(0.,0.707106781186547,0.707106781186548));
#16472=DIRECTION('ref_axis',(1.,0.,0.));
#16473=DIRECTION('',(-0.577350269189626,0.577350269189626,-0.577350269189625));
#16474=DIRECTION('',(1.,0.,0.));
#16475=DIRECTION('',(0.591591578932266,0.570096221587387,-0.570096221587386));
#16476=DIRECTION('center_axis',(0.,0.707106781186548,-0.707106781186548));
#16477=DIRECTION('ref_axis',(-1.,0.,0.));
#16478=DIRECTION('',(0.577350269189626,0.577350269189626,0.577350269189626));
#16479=DIRECTION('',(-1.,0.,0.));
#16480=DIRECTION('center_axis',(0.,0.,-1.));
#16481=DIRECTION('ref_axis',(-1.,0.,0.));
#16482=DIRECTION('',(0.,1.,0.));
#16483=DIRECTION('',(1.,0.,0.));
#16484=DIRECTION('',(0.,1.,0.));
#16485=DIRECTION('center_axis',(0.577350269189626,0.577350269189626,0.577350269189626));
#16486=DIRECTION('ref_axis',(0.707106781186548,0.,-0.707106781186547));
#16487=DIRECTION('',(0.,0.707106781186548,-0.707106781186547));
#16488=DIRECTION('',(-0.707106781186548,0.,0.707106781186547));
#16489=DIRECTION('',(0.707106781186547,-0.707106781186547,0.));
#16490=DIRECTION('center_axis',(0.707106781186547,0.,0.707106781186548));
#16491=DIRECTION('ref_axis',(0.707106781186548,0.,-0.707106781186547));
#16492=DIRECTION('',(0.577350269189626,0.577350269189626,-0.577350269189625));
#16493=DIRECTION('',(0.,1.,0.));
#16494=DIRECTION('',(0.,-1.,0.));
#16495=DIRECTION('',(0.577350269189626,-0.577350269189626,-0.577350269189625));
#16496=DIRECTION('center_axis',(0.707106781186548,0.707106781186548,0.));
#16497=DIRECTION('ref_axis',(0.,0.,-1.));
#16498=DIRECTION('',(-0.707106781186547,0.707106781186547,0.));
#16499=DIRECTION('',(0.,0.,-1.));
#16500=DIRECTION('center_axis',(0.,-1.,0.));
#16501=DIRECTION('ref_axis',(0.707106781186546,0.,-0.707106781186549));
#16502=DIRECTION('center_axis',(0.,1.,0.));
#16503=DIRECTION('ref_axis',(0.707106781186546,0.,-0.707106781186549));
#16504=DIRECTION('',(0.,0.707106781186545,0.70710678118655));
#16505=DIRECTION('center_axis',(0.,0.707106781186548,-0.707106781186548));
#16506=DIRECTION('ref_axis',(-1.,0.,0.));
#16507=DIRECTION('',(0.577350269189626,-0.577350269189626,-0.577350269189626));
#16508=DIRECTION('',(-1.,0.,0.));
#16509=DIRECTION('center_axis',(0.,0.707106781186547,0.707106781186548));
#16510=DIRECTION('ref_axis',(1.,0.,0.));
#16511=DIRECTION('',(0.591591578932266,-0.570096221587387,0.570096221587386));
#16512=DIRECTION('',(1.,0.,0.));
#16513=DIRECTION('center_axis',(0.,1.,0.));
#16514=DIRECTION('ref_axis',(0.707106781186546,0.,-0.707106781186549));
#16515=DIRECTION('',(0.,-1.,0.));
#16516=DIRECTION('center_axis',(0.,-1.,0.));
#16517=DIRECTION('ref_axis',(0.707106781186546,0.,-0.707106781186549));
#16518=DIRECTION('',(0.,1.,0.));
#16519=DIRECTION('center_axis',(1.,0.,0.));
#16520=DIRECTION('ref_axis',(0.,0.,-1.));
#16521=DIRECTION('',(0.,0.,1.));
#16522=DIRECTION('center_axis',(0.707106781186548,-0.707106781186548,0.));
#16523=DIRECTION('ref_axis',(0.,0.,-1.));
#16524=DIRECTION('',(0.577350269189626,0.577350269189626,0.577350269189625));
#16525=DIRECTION('',(0.707106781186547,0.707106781186547,0.));
#16526=DIRECTION('center_axis',(0.,-0.707106781186547,0.707106781186548));
#16527=DIRECTION('ref_axis',(1.,0.,0.));
#16528=DIRECTION('',(-1.,0.,0.));
#16529=DIRECTION('',(-0.591591578932266,-0.570096221587387,-0.570096221587386));
#16530=DIRECTION('center_axis',(0.,0.,1.));
#16531=DIRECTION('ref_axis',(1.,0.,0.));
#16532=DIRECTION('',(0.,1.,0.));
#16533=DIRECTION('center_axis',(0.,0.,-1.));
#16534=DIRECTION('ref_axis',(1.,0.,0.));
#16535=DIRECTION('center_axis',(-0.693904010166723,0.,0.720067513969725));
#16536=DIRECTION('ref_axis',(0.720067513969725,0.,0.693904010166723));
#16537=DIRECTION('',(0.,-1.,0.));
#16538=DIRECTION('center_axis',(0.,1.,0.));
#16539=DIRECTION('ref_axis',(0.707106781186546,0.,-0.707106781186549));
#16540=DIRECTION('',(0.,0.707106781186545,-0.70710678118655));
#16541=DIRECTION('center_axis',(0.,-0.707106781186548,-0.707106781186548));
#16542=DIRECTION('ref_axis',(-1.,0.,0.));
#16543=DIRECTION('',(1.,0.,0.));
#16544=DIRECTION('',(0.577350269189625,0.577350269189625,-0.577350269189627));
#16545=DIRECTION('center_axis',(0.707106781186548,0.707106781186548,0.));
#16546=DIRECTION('ref_axis',(0.,0.,-1.));
#16547=DIRECTION('',(0.,0.,-1.));
#16548=DIRECTION('',(-0.707106781186547,0.707106781186547,0.));
#16549=DIRECTION('center_axis',(-1.,0.,0.));
#16550=DIRECTION('ref_axis',(0.,0.707106781186547,-0.707106781186548));
#16551=DIRECTION('',(-0.707106781186551,4.08878244448901E-16,-0.707106781186544));
#16552=DIRECTION('center_axis',(1.,0.,0.));
#16553=DIRECTION('ref_axis',(0.,0.707106781186547,-0.707106781186548));
#16554=DIRECTION('center_axis',(-1.,0.,0.));
#16555=DIRECTION('ref_axis',(0.,0.707106781186547,-0.707106781186548));
#16556=DIRECTION('center_axis',(0.707106781186548,0.,-0.707106781186548));
#16557=DIRECTION('ref_axis',(-0.707106781186548,0.,-0.707106781186548));
#16558=DIRECTION('',(0.,-1.,0.));
#16559=DIRECTION('',(-0.707106781186547,0.,-0.707106781186547));
#16560=DIRECTION('',(0.,1.,0.));
#16561=DIRECTION('center_axis',(-1.,0.,0.));
#16562=DIRECTION('ref_axis',(0.,-0.707106781186547,-0.707106781186548));
#16563=DIRECTION('',(-0.707106781186549,-0.707106781186546,0.));
#16564=DIRECTION('center_axis',(1.,0.,0.));
#16565=DIRECTION('ref_axis',(0.,-0.707106781186547,-0.707106781186548));
#16566=DIRECTION('center_axis',(-1.,0.,0.));
#16567=DIRECTION('ref_axis',(0.,-0.707106781186547,-0.707106781186548));
#16568=DIRECTION('center_axis',(0.707106781186548,-0.707106781186548,0.));
#16569=DIRECTION('ref_axis',(0.,0.,-1.));
#16570=DIRECTION('',(0.,0.,1.));
#16571=DIRECTION('center_axis',(0.,0.,-1.));
#16572=DIRECTION('ref_axis',(-1.,0.,0.));
#16573=DIRECTION('',(0.,1.,0.));
#16574=DIRECTION('center_axis',(0.,0.,1.));
#16575=DIRECTION('ref_axis',(1.,0.,0.));
#16576=DIRECTION('center_axis',(1.,0.,0.));
#16577=DIRECTION('ref_axis',(0.,0.,-1.));
#16578=DIRECTION('center_axis',(-1.,0.,0.));
#16579=DIRECTION('ref_axis',(0.,0.,-1.));
#16580=DIRECTION('center_axis',(-0.707106781186548,-0.707106781186548,0.));
#16581=DIRECTION('ref_axis',(0.,0.,1.));
#16582=DIRECTION('',(0.,0.,-1.));
#16583=DIRECTION('',(0.707106781186547,-0.707106781186547,0.));
#16584=DIRECTION('',(-0.577350269189626,0.577350269189626,-0.577350269189626));
#16585=DIRECTION('center_axis',(0.,-0.707106781186548,-0.707106781186548));
#16586=DIRECTION('ref_axis',(-1.,0.,0.));
#16587=DIRECTION('center_axis',(1.,0.,0.));
#16588=DIRECTION('ref_axis',(0.,-0.707106781186547,-0.707106781186548));
#16589=DIRECTION('',(0.707106781186551,-4.08878244448901E-16,-0.707106781186544));
#16590=DIRECTION('center_axis',(-1.,0.,0.));
#16591=DIRECTION('ref_axis',(0.,-0.707106781186547,-0.707106781186548));
#16592=DIRECTION('center_axis',(1.,0.,0.));
#16593=DIRECTION('ref_axis',(0.,-0.707106781186547,-0.707106781186548));
#16594=DIRECTION('center_axis',(-0.707106781186548,0.,-0.707106781186548));
#16595=DIRECTION('ref_axis',(-0.707106781186548,0.,0.707106781186548));
#16596=DIRECTION('',(0.707106781186547,0.,-0.707106781186547));
#16597=DIRECTION('',(0.,-1.,0.));
#16598=DIRECTION('',(0.,1.,0.));
#16599=DIRECTION('center_axis',(1.,0.,0.));
#16600=DIRECTION('ref_axis',(0.,0.707106781186547,-0.707106781186548));
#16601=DIRECTION('',(0.707106781186549,0.707106781186546,0.));
#16602=DIRECTION('center_axis',(-1.,0.,0.));
#16603=DIRECTION('ref_axis',(0.,0.707106781186547,-0.707106781186548));
#16604=DIRECTION('center_axis',(1.,0.,0.));
#16605=DIRECTION('ref_axis',(0.,0.707106781186547,-0.707106781186548));
#16606=DIRECTION('center_axis',(-0.707106781186548,0.707106781186548,0.));
#16607=DIRECTION('ref_axis',(0.,0.,1.));
#16608=DIRECTION('',(0.,0.,1.));
#16609=DIRECTION('center_axis',(-1.,0.,0.));
#16610=DIRECTION('ref_axis',(0.,0.,1.));
#16611=DIRECTION('center_axis',(1.,0.,0.));
#16612=DIRECTION('ref_axis',(0.,0.,-1.));
#16613=DIRECTION('center_axis',(0.,-0.707106781186548,-0.707106781186548));
#16614=DIRECTION('ref_axis',(-1.,0.,0.));
#16615=DIRECTION('center_axis',(0.,-0.707106781186547,0.707106781186548));
#16616=DIRECTION('ref_axis',(1.,0.,0.));
#16617=DIRECTION('',(-0.591591578932266,0.570096221587387,0.570096221587386));
#16618=DIRECTION('',(-1.,0.,0.));
#16619=DIRECTION('',(-0.577350269189626,-0.577350269189626,-0.577350269189625));
#16620=DIRECTION('center_axis',(-0.707106781186547,0.,0.707106781186548));
#16621=DIRECTION('ref_axis',(0.707106781186548,0.,0.707106781186547));
#16622=DIRECTION('',(0.,1.,0.));
#16623=DIRECTION('',(0.,-1.,0.));
#16624=DIRECTION('center_axis',(0.,-1.,0.));
#16625=DIRECTION('ref_axis',(1.,0.,0.));
#16626=DIRECTION('center_axis',(0.,1.,0.));
#16627=DIRECTION('ref_axis',(1.,0.,0.));
#16628=DIRECTION('center_axis',(-1.,0.,0.));
#16629=DIRECTION('ref_axis',(0.,0.,1.));
#16630=DIRECTION('',(0.,1.,0.));
#16631=DIRECTION('center_axis',(0.,1.,0.));
#16632=DIRECTION('ref_axis',(1.,0.,0.));
#16633=DIRECTION('center_axis',(0.,-1.,0.));
#16634=DIRECTION('ref_axis',(1.,0.,0.));
#16635=DIRECTION('center_axis',(0.,1.,0.));
#16636=DIRECTION('ref_axis',(1.,0.,0.));
#16637=DIRECTION('',(0.,1.,0.));
#16638=DIRECTION('',(0.,1.,0.));
#16639=DIRECTION('center_axis',(0.,-1.,0.));
#16640=DIRECTION('ref_axis',(1.,0.,0.));
#16641=DIRECTION('',(0.,-1.,0.));
#16642=DIRECTION('center_axis',(0.,1.,0.));
#16643=DIRECTION('ref_axis',(1.,0.,0.));
#16644=DIRECTION('center_axis',(0.693904010166723,0.,0.720067513969725));
#16645=DIRECTION('ref_axis',(0.720067513969725,0.,-0.693904010166723));
#16646=DIRECTION('',(0.,-1.,0.));
#16647=DIRECTION('center_axis',(0.993041625297607,0.,-0.117763875727185));
#16648=DIRECTION('ref_axis',(-0.117763875727185,0.,-0.993041625297607));
#16649=DIRECTION('',(0.,1.,0.));
#16650=DIRECTION('center_axis',(-0.993041625297607,0.,-0.117763875727185));
#16651=DIRECTION('ref_axis',(-0.117763875727185,0.,0.993041625297607));
#16652=DIRECTION('',(0.,-1.,0.));
#16653=DIRECTION('center_axis',(0.,-1.,0.));
#16654=DIRECTION('ref_axis',(1.,0.,0.));
#16655=DIRECTION('center_axis',(0.,-1.,0.));
#16656=DIRECTION('ref_axis',(1.,0.,0.));
#16657=DIRECTION('center_axis',(0.,1.,0.));
#16658=DIRECTION('ref_axis',(1.,0.,0.));
#16659=DIRECTION('center_axis',(0.,1.,0.));
#16660=DIRECTION('ref_axis',(1.,0.,0.));
#16661=DIRECTION('center_axis',(0.,1.,0.));
#16662=DIRECTION('ref_axis',(1.,0.,0.));
#16663=DIRECTION('',(-1.,0.,0.));
#16664=DIRECTION('',(0.,0.,1.));
#16665=DIRECTION('center_axis',(0.,-1.,0.));
#16666=DIRECTION('ref_axis',(1.,0.,0.));
#16667=DIRECTION('',(0.,0.,-1.));
#16668=DIRECTION('',(-1.,0.,0.));
#16669=DIRECTION('center_axis',(0.,0.,1.));
#16670=DIRECTION('ref_axis',(1.,0.,0.));
#16671=DIRECTION('',(1.,0.,0.));
#16672=DIRECTION('',(0.,1.,0.));
#16673=DIRECTION('center_axis',(0.55942034633874,0.,-0.828884115001756));
#16674=DIRECTION('ref_axis',(-0.828884115001756,0.,-0.55942034633874));
#16675=DIRECTION('',(0.,1.,0.));
#16676=DIRECTION('',(0.,-1.,0.));
#16677=DIRECTION('center_axis',(-0.55942034633874,0.,-0.828884115001756));
#16678=DIRECTION('ref_axis',(-0.828884115001756,0.,0.55942034633874));
#16679=DIRECTION('',(0.,-1.,0.));
#16680=DIRECTION('',(0.,1.,0.));
#16681=DIRECTION('center_axis',(0.,-1.,0.));
#16682=DIRECTION('ref_axis',(1.,0.,0.));
#16683=DIRECTION('center_axis',(0.,1.,0.));
#16684=DIRECTION('ref_axis',(1.,0.,0.));
#16685=DIRECTION('center_axis',(0.,1.,0.));
#16686=DIRECTION('ref_axis',(1.,0.,0.));
#16687=DIRECTION('center_axis',(0.,-1.,0.));
#16688=DIRECTION('ref_axis',(1.,0.,0.));
#16689=DIRECTION('center_axis',(0.,1.,0.));
#16690=DIRECTION('ref_axis',(1.,0.,0.));
#16691=DIRECTION('center_axis',(0.,1.,0.));
#16692=DIRECTION('ref_axis',(0.,0.,1.));
#16693=DIRECTION('',(1.,0.,0.));
#16694=DIRECTION('',(0.,0.,1.));
#16695=DIRECTION('',(0.,0.,-1.));
#16696=DIRECTION('center_axis',(1.,0.,0.));
#16697=DIRECTION('ref_axis',(0.,0.,-1.));
#16698=DIRECTION('center_axis',(0.,1.,0.));
#16699=DIRECTION('ref_axis',(1.,0.,0.));
#16700=DIRECTION('center_axis',(0.,1.,0.));
#16701=DIRECTION('ref_axis',(1.,0.,0.));
#16702=DIRECTION('center_axis',(0.,-1.,0.));
#16703=DIRECTION('ref_axis',(1.,0.,0.));
#16704=DIRECTION('center_axis',(0.,-1.,0.));
#16705=DIRECTION('ref_axis',(1.,0.,0.));
#16706=DIRECTION('center_axis',(0.,0.,1.));
#16707=DIRECTION('ref_axis',(1.,0.,0.));
#16708=DIRECTION('center_axis',(0.,0.,-1.));
#16709=DIRECTION('ref_axis',(1.,0.,0.));
#16710=DIRECTION('center_axis',(0.,1.,0.));
#16711=DIRECTION('ref_axis',(1.,0.,0.));
#16712=DIRECTION('center_axis',(-1.,0.,0.));
#16713=DIRECTION('ref_axis',(0.,0.,1.));
#16714=DIRECTION('',(0.,1.,0.));
#16715=DIRECTION('center_axis',(0.,0.,1.));
#16716=DIRECTION('ref_axis',(1.,0.,0.));
#16717=DIRECTION('center_axis',(0.,0.,-1.));
#16718=DIRECTION('ref_axis',(1.,0.,0.));
#16719=DIRECTION('',(0.,0.,-1.));
#16720=DIRECTION('center_axis',(0.,0.,-1.));
#16721=DIRECTION('ref_axis',(1.,0.,0.));
#16722=DIRECTION('',(0.,0.,-1.));
#16723=DIRECTION('center_axis',(0.,0.,1.));
#16724=DIRECTION('ref_axis',(1.,0.,0.));
#16725=DIRECTION('center_axis',(1.,0.,0.));
#16726=DIRECTION('ref_axis',(0.,0.,-1.));
#16727=DIRECTION('center_axis',(1.,0.,0.));
#16728=DIRECTION('ref_axis',(0.,0.,-1.));
#16729=DIRECTION('',(1.,0.,0.));
#16730=DIRECTION('center_axis',(-1.,0.,0.));
#16731=DIRECTION('ref_axis',(0.,0.,-1.));
#16732=DIRECTION('',(-1.,0.,0.));
#16733=DIRECTION('center_axis',(1.,0.,0.));
#16734=DIRECTION('ref_axis',(0.,-0.707106781186547,-0.707106781186548));
#16735=DIRECTION('',(1.,0.,0.));
#16736=DIRECTION('center_axis',(-1.,0.,0.));
#16737=DIRECTION('ref_axis',(0.,0.707106781186547,-0.707106781186548));
#16738=DIRECTION('',(-1.,0.,0.));
#16739=DIRECTION('center_axis',(0.,1.,0.));
#16740=DIRECTION('ref_axis',(-0.707106781186549,0.,-0.707106781186546));
#16741=DIRECTION('',(0.,-1.,0.));
#16742=DIRECTION('center_axis',(0.,0.,-1.));
#16743=DIRECTION('ref_axis',(-1.,0.,0.));
#16744=DIRECTION('',(0.,1.,0.));
#16745=DIRECTION('center_axis',(0.,0.,-1.));
#16746=DIRECTION('ref_axis',(-1.,0.,0.));
#16747=DIRECTION('center_axis',(-1.,0.,0.));
#16748=DIRECTION('ref_axis',(0.,0.,1.));
#16749=DIRECTION('axis',(0.,0.,1.));
#16750=DIRECTION('refdir',(1.,0.,0.));
#16751=DIRECTION('center_axis',(0.707106781186549,0.707106781186546,0.));
#16752=DIRECTION('ref_axis',(0.,0.,-1.));
#16753=DIRECTION('',(0.707106781186546,-0.707106781186549,0.));
#16754=DIRECTION('',(0.,0.,1.));
#16755=DIRECTION('',(0.707106781186547,-0.707106781186548,0.));
#16756=DIRECTION('',(0.,0.,-1.));
#16757=DIRECTION('center_axis',(-1.,0.,0.));
#16758=DIRECTION('ref_axis',(0.,1.,7.40148683083438E-16));
#16759=DIRECTION('',(0.707106781186547,0.707106781186548,0.));
#16760=DIRECTION('center_axis',(-1.,0.,0.));
#16761=DIRECTION('ref_axis',(0.,1.,7.40148683083438E-16));
#16762=DIRECTION('center_axis',(1.,0.,0.));
#16763=DIRECTION('ref_axis',(0.,1.,7.40148683083438E-16));
#16764=DIRECTION('center_axis',(0.707106781186549,-0.707106781186546,0.));
#16765=DIRECTION('ref_axis',(0.,0.,-1.));
#16766=DIRECTION('',(-0.707106781186546,-0.707106781186549,0.));
#16767=DIRECTION('',(0.,0.,1.));
#16768=DIRECTION('',(0.,0.,-1.));
#16769=DIRECTION('center_axis',(0.,-1.,0.));
#16770=DIRECTION('ref_axis',(0.,0.,-1.));
#16771=DIRECTION('',(1.,0.,0.));
#16772=DIRECTION('',(0.,0.,1.));
#16773=DIRECTION('',(-1.,0.,0.));
#16774=DIRECTION('center_axis',(1.,0.,0.));
#16775=DIRECTION('ref_axis',(0.,1.,7.40148683083438E-16));
#16776=DIRECTION('',(1.,0.,0.));
#16777=DIRECTION('center_axis',(-1.,0.,0.));
#16778=DIRECTION('ref_axis',(0.,1.,7.40148683083438E-16));
#16779=DIRECTION('center_axis',(0.,1.,0.));
#16780=DIRECTION('ref_axis',(0.,0.,1.));
#16781=DIRECTION('',(1.,0.,0.));
#16782=DIRECTION('',(0.,0.,-1.));
#16783=DIRECTION('center_axis',(-0.707106781186549,0.707106781186546,0.));
#16784=DIRECTION('ref_axis',(0.,0.,1.));
#16785=DIRECTION('',(0.707106781186546,0.707106781186549,0.));
#16786=DIRECTION('',(0.,0.,1.));
#16787=DIRECTION('',(0.707106781186547,0.707106781186548,0.));
#16788=DIRECTION('center_axis',(1.,0.,0.));
#16789=DIRECTION('ref_axis',(0.,1.,7.40148683083438E-16));
#16790=DIRECTION('',(0.707106781186547,-0.707106781186548,0.));
#16791=DIRECTION('center_axis',(1.,0.,0.));
#16792=DIRECTION('ref_axis',(0.,1.,7.40148683083438E-16));
#16793=DIRECTION('center_axis',(-0.707106781186549,-0.707106781186546,0.));
#16794=DIRECTION('ref_axis',(0.,0.,1.));
#16795=DIRECTION('',(-0.707106781186546,0.707106781186549,0.));
#16796=DIRECTION('',(0.,0.,-1.));
#16797=DIRECTION('center_axis',(1.,0.,0.));
#16798=DIRECTION('ref_axis',(0.,0.,-1.));
#16799=DIRECTION('',(0.,1.,0.));
#16800=DIRECTION('',(0.,-0.866025403784439,-0.499999999999999));
#16801=DIRECTION('',(0.,-4.062597224754E-16,-1.));
#16802=DIRECTION('',(0.,0.866025403784439,-0.5));
#16803=DIRECTION('',(0.,0.866025403784439,0.5));
#16804=DIRECTION('',(0.,-1.354199074918E-16,1.));
#16805=DIRECTION('',(0.,-0.866025403784439,0.499999999999999));
#16806=DIRECTION('center_axis',(-0.707106781186549,-0.707106781186546,0.));
#16807=DIRECTION('ref_axis',(0.,0.,1.));
#16808=DIRECTION('',(-0.707106781186546,0.707106781186549,0.));
#16809=DIRECTION('',(0.,0.,1.));
#16810=DIRECTION('',(-0.707106781186546,0.707106781186549,0.));
#16811=DIRECTION('',(0.,0.,-1.));
#16812=DIRECTION('center_axis',(1.,0.,0.));
#16813=DIRECTION('ref_axis',(0.,1.,7.40148683083438E-16));
#16814=DIRECTION('',(-0.707106781186548,-0.707106781186548,0.));
#16815=DIRECTION('center_axis',(1.,0.,0.));
#16816=DIRECTION('ref_axis',(0.,1.,7.40148683083438E-16));
#16817=DIRECTION('center_axis',(-1.,0.,0.));
#16818=DIRECTION('ref_axis',(0.,1.,7.40148683083438E-16));
#16819=DIRECTION('center_axis',(-0.707106781186549,0.707106781186546,0.));
#16820=DIRECTION('ref_axis',(0.,0.,1.));
#16821=DIRECTION('',(0.707106781186546,0.707106781186549,0.));
#16822=DIRECTION('',(0.,0.,1.));
#16823=DIRECTION('',(0.,0.,-1.));
#16824=DIRECTION('center_axis',(0.,1.,0.));
#16825=DIRECTION('ref_axis',(0.,0.,-1.));
#16826=DIRECTION('',(-1.,0.,0.));
#16827=DIRECTION('',(0.,0.,1.));
#16828=DIRECTION('',(1.,0.,0.));
#16829=DIRECTION('center_axis',(-1.,0.,0.));
#16830=DIRECTION('ref_axis',(0.,1.,7.40148683083438E-16));
#16831=DIRECTION('',(-1.,0.,0.));
#16832=DIRECTION('center_axis',(1.,0.,0.));
#16833=DIRECTION('ref_axis',(0.,1.,7.40148683083438E-16));
#16834=DIRECTION('center_axis',(0.,-1.,0.));
#16835=DIRECTION('ref_axis',(0.,0.,1.));
#16836=DIRECTION('',(-1.,0.,0.));
#16837=DIRECTION('',(0.,0.,-1.));
#16838=DIRECTION('center_axis',(0.577350269189626,-0.577350269189625,0.577350269189626));
#16839=DIRECTION('ref_axis',(0.707106781186548,0.,-0.707106781186548));
#16840=DIRECTION('',(0.,0.707106781186549,0.707106781186546));
#16841=DIRECTION('',(-0.707106781186546,-0.707106781186549,0.));
#16842=DIRECTION('',(0.707106781186548,0.,-0.707106781186548));
#16843=DIRECTION('center_axis',(0.707106781186549,-0.707106781186546,0.));
#16844=DIRECTION('ref_axis',(0.,0.,-1.));
#16845=DIRECTION('',(-0.707106781186546,-0.707106781186549,0.));
#16846=DIRECTION('',(0.,0.,1.));
#16847=DIRECTION('',(0.,0.,-1.));
#16848=DIRECTION('center_axis',(0.707106781186548,0.,0.707106781186548));
#16849=DIRECTION('ref_axis',(0.707106781186548,0.,-0.707106781186548));
#16850=DIRECTION('',(-0.577350269189627,-0.577350269189624,0.577350269189627));
#16851=DIRECTION('',(0.,-1.,0.));
#16852=DIRECTION('',(0.,1.,0.));
#16853=DIRECTION('',(-0.577350269189625,0.577350269189628,0.577350269189625));
#16854=DIRECTION('center_axis',(0.,-0.707106781186546,0.707106781186549));
#16855=DIRECTION('ref_axis',(1.,0.,0.));
#16856=DIRECTION('',(0.577350269189626,-0.577350269189627,-0.577350269189625));
#16857=DIRECTION('',(1.,0.,0.));
#16858=DIRECTION('',(-1.,0.,0.));
#16859=DIRECTION('',(-0.577350269189627,-0.577350269189626,-0.577350269189624));
#16860=DIRECTION('center_axis',(1.,0.,0.));
#16861=DIRECTION('ref_axis',(0.,1.,0.));
#16862=DIRECTION('',(0.,-1.,0.));
#16863=DIRECTION('',(0.,0.,-1.));
#16864=DIRECTION('center_axis',(0.,-1.,0.));
#16865=DIRECTION('ref_axis',(1.,0.,0.));
#16866=DIRECTION('',(0.,0.,1.));
#16867=DIRECTION('',(-1.,0.,0.));
#16868=DIRECTION('center_axis',(-0.707106781186548,-0.707106781186547,0.));
#16869=DIRECTION('ref_axis',(0.,0.,1.));
#16870=DIRECTION('',(-0.577350269189625,0.577350269189627,-0.577350269189625));
#16871=DIRECTION('',(0.,0.,-1.));
#16872=DIRECTION('',(-0.707106781186547,0.707106781186548,0.));
#16873=DIRECTION('center_axis',(1.,0.,0.));
#16874=DIRECTION('ref_axis',(0.,0.,-1.));
#16875=DIRECTION('center_axis',(1.,0.,0.));
#16876=DIRECTION('ref_axis',(0.,0.,-1.));
#16877=DIRECTION('',(-0.707106781186548,8.65956056235493E-17,-0.707106781186548));
#16878=DIRECTION('center_axis',(-1.,0.,0.));
#16879=DIRECTION('ref_axis',(0.,0.,-1.));
#16880=DIRECTION('center_axis',(-1.,0.,0.));
#16881=DIRECTION('ref_axis',(0.,0.,-1.));
#16882=DIRECTION('',(-1.,0.,0.));
#16883=DIRECTION('center_axis',(1.,0.,0.));
#16884=DIRECTION('ref_axis',(0.,0.,-1.));
#16885=DIRECTION('center_axis',(1.,0.,0.));
#16886=DIRECTION('ref_axis',(0.,0.,-1.));
#16887=DIRECTION('',(0.,-1.,0.));
#16888=DIRECTION('center_axis',(-1.,0.,0.));
#16889=DIRECTION('ref_axis',(0.,0.,-1.));
#16890=DIRECTION('center_axis',(-1.,0.,0.));
#16891=DIRECTION('ref_axis',(0.,0.,-1.));
#16892=DIRECTION('',(0.707106781186548,-8.65956056235493E-17,-0.707106781186548));
#16893=DIRECTION('center_axis',(1.,0.,0.));
#16894=DIRECTION('ref_axis',(0.,0.,-1.));
#16895=DIRECTION('center_axis',(1.,0.,0.));
#16896=DIRECTION('ref_axis',(0.,0.,-1.));
#16897=DIRECTION('',(1.,0.,0.));
#16898=DIRECTION('center_axis',(-1.,0.,0.));
#16899=DIRECTION('ref_axis',(0.,0.,-1.));
#16900=DIRECTION('center_axis',(1.,0.,0.));
#16901=DIRECTION('ref_axis',(0.,0.,-1.));
#16902=DIRECTION('',(0.,1.,0.));
#16903=DIRECTION('center_axis',(-1.,0.,0.));
#16904=DIRECTION('ref_axis',(0.,0.,-1.));
#16905=DIRECTION('',(-0.707106781186548,-8.65956056235493E-17,0.707106781186548));
#16906=DIRECTION('center_axis',(-1.,0.,0.));
#16907=DIRECTION('ref_axis',(0.,0.,-1.));
#16908=DIRECTION('center_axis',(1.,0.,0.));
#16909=DIRECTION('ref_axis',(0.,0.,-1.));
#16910=DIRECTION('',(0.,4.062597224754E-16,1.));
#16911=DIRECTION('',(0.,0.866025403784439,0.499999999999999));
#16912=DIRECTION('',(0.,0.866025403784439,-0.499999999999999));
#16913=DIRECTION('',(0.,1.354199074918E-16,-1.));
#16914=DIRECTION('',(0.,-0.866025403784439,-0.5));
#16915=DIRECTION('',(0.,-0.866025403784439,0.5));
#16916=DIRECTION('center_axis',(-0.70710678118655,0.353553390593272,-0.612372435695792));
#16917=DIRECTION('ref_axis',(-0.654653670707974,0.,0.755928946018457));
#16918=DIRECTION('',(0.654653670707975,-3.98171761111234E-16,-0.755928946018456));
#16919=DIRECTION('',(0.,-0.866025403784439,-0.5));
#16920=DIRECTION('',(0.654653670707976,0.654653670707976,-0.377964473009231));
#16921=DIRECTION('center_axis',(-0.70710678118655,-0.353553390593272,-0.612372435695792));
#16922=DIRECTION('ref_axis',(-0.654653670707974,0.,0.755928946018457));
#16923=DIRECTION('',(0.654653670707975,-0.654653670707977,-0.377964473009231));
#16924=DIRECTION('',(0.,-0.866025403784439,0.5));
#16925=DIRECTION('center_axis',(-0.707106781186554,-0.35355339059327,0.612372435695789));
#16926=DIRECTION('ref_axis',(0.654653670707971,0.,0.75592894601846));
#16927=DIRECTION('',(0.654653670707972,-4.61997734366925E-15,0.755928946018459));
#16928=DIRECTION('',(0.,0.866025403784439,0.499999999999999));
#16929=DIRECTION('',(-0.654653670707974,0.654653670707975,-0.377964473009236));
#16930=DIRECTION('center_axis',(-0.707106781186551,0.353553390593272,0.612372435695792));
#16931=DIRECTION('ref_axis',(0.654653670707974,0.,0.755928946018457));
#16932=DIRECTION('',(0.,0.866025403784439,-0.499999999999999));
#16933=DIRECTION('',(0.654653670707974,0.654653670707975,0.377964473009236));
#16934=DIRECTION('center_axis',(-0.707106781186548,-0.707106781186547,2.8726900468532E-16));
#16935=DIRECTION('ref_axis',(4.062597224754E-16,0.,1.));
#16936=DIRECTION('',(0.,4.062597224754E-16,1.));
#16937=DIRECTION('center_axis',(-0.707106781186548,0.707106781186547,9.57563348951068E-17));
#16938=DIRECTION('ref_axis',(1.354199074918E-16,0.,1.));
#16939=DIRECTION('',(0.,1.354199074918E-16,-1.));
#16940=DIRECTION('center_axis',(0.,0.5,0.866025403784439));
#16941=DIRECTION('ref_axis',(0.,-0.866025403784439,0.5));
#16942=DIRECTION('',(1.,0.,0.));
#16943=DIRECTION('',(1.,0.,0.));
#16944=DIRECTION('center_axis',(0.,1.,-4.062597224754E-16));
#16945=DIRECTION('ref_axis',(0.,4.062597224754E-16,1.));
#16946=DIRECTION('',(1.,0.,0.));
#16947=DIRECTION('center_axis',(0.,0.499999999999999,-0.866025403784439));
#16948=DIRECTION('ref_axis',(0.,0.866025403784439,0.499999999999999));
#16949=DIRECTION('',(1.,0.,0.));
#16950=DIRECTION('center_axis',(1.,0.,0.));
#16951=DIRECTION('ref_axis',(0.,0.,-1.));
#16952=DIRECTION('',(0.707106781186548,8.65956056235493E-17,0.707106781186548));
#16953=DIRECTION('center_axis',(1.,0.,0.));
#16954=DIRECTION('ref_axis',(0.,0.,-1.));
#16955=DIRECTION('center_axis',(-1.,0.,0.));
#16956=DIRECTION('ref_axis',(0.,0.,1.));
#16957=DIRECTION('',(0.,-4.062597224754E-16,-1.));
#16958=DIRECTION('',(0.,0.866025403784439,-0.5));
#16959=DIRECTION('',(0.,0.866025403784439,0.5));
#16960=DIRECTION('',(0.,-1.354199074918E-16,1.));
#16961=DIRECTION('',(0.,-0.866025403784439,0.499999999999999));
#16962=DIRECTION('',(0.,-0.866025403784439,-0.499999999999999));
#16963=DIRECTION('center_axis',(0.707106781186549,0.707106781186546,0.));
#16964=DIRECTION('ref_axis',(0.,0.,-1.));
#16965=DIRECTION('',(0.707106781186546,-0.707106781186549,0.));
#16966=DIRECTION('',(0.707106781186547,-0.707106781186548,0.));
#16967=DIRECTION('',(0.,0.,-1.));
#16968=DIRECTION('center_axis',(-1.,0.,0.));
#16969=DIRECTION('ref_axis',(0.,1.,7.40148683083438E-16));
#16970=DIRECTION('',(0.707106781186547,0.707106781186548,0.));
#16971=DIRECTION('center_axis',(-1.,0.,0.));
#16972=DIRECTION('ref_axis',(0.,1.,7.40148683083438E-16));
#16973=DIRECTION('center_axis',(0.707106781186549,-0.707106781186546,0.));
#16974=DIRECTION('ref_axis',(0.,0.,-1.));
#16975=DIRECTION('',(-0.707106781186546,-0.707106781186549,0.));
#16976=DIRECTION('',(0.,0.,1.));
#16977=DIRECTION('center_axis',(0.70710678118655,0.353553390593272,0.612372435695793));
#16978=DIRECTION('ref_axis',(0.654653670707975,0.,-0.755928946018457));
#16979=DIRECTION('',(0.,0.866025403784439,-0.499999999999999));
#16980=DIRECTION('',(-0.654653670707975,-3.8931657652939E-15,0.755928946018456));
#16981=DIRECTION('',(0.,-0.866025403784439,0.499999999999999));
#16982=DIRECTION('',(-0.654653670707975,0.654653670707977,0.377964473009231));
#16983=DIRECTION('center_axis',(0.707106781186551,-0.353553390593272,0.612372435695792));
#16984=DIRECTION('ref_axis',(0.654653670707974,0.,-0.755928946018457));
#16985=DIRECTION('',(0.,0.866025403784439,0.499999999999999));
#16986=DIRECTION('',(-0.654653670707974,-0.654653670707975,0.377964473009236));
#16987=DIRECTION('',(0.,-0.866025403784439,-0.499999999999999));
#16988=DIRECTION('center_axis',(0.70710678118655,-0.353553390593272,-0.612372435695792));
#16989=DIRECTION('ref_axis',(-0.654653670707974,0.,-0.755928946018457));
#16990=DIRECTION('',(0.,-0.866025403784439,0.5));
#16991=DIRECTION('',(-0.654653670707975,3.28639817264138E-16,-0.755928946018456));
#16992=DIRECTION('',(0.,0.866025403784439,-0.5));
#16993=DIRECTION('',(0.654653670707975,0.654653670707977,0.377964473009231));
#16994=DIRECTION('center_axis',(0.70710678118655,0.353553390593272,-0.612372435695792));
#16995=DIRECTION('ref_axis',(-0.654653670707974,0.,-0.755928946018457));
#16996=DIRECTION('',(0.,0.866025403784439,0.5));
#16997=DIRECTION('',(0.,-0.866025403784439,-0.5));
#16998=DIRECTION('',(-0.654653670707975,0.654653670707977,-0.377964473009231));
#16999=DIRECTION('center_axis',(0.707106781186548,-0.707106781186547,2.8726900468532E-16));
#17000=DIRECTION('ref_axis',(4.062597224754E-16,0.,-1.));
#17001=DIRECTION('',(0.,4.062597224754E-16,1.));
#17002=DIRECTION('',(0.,-4.062597224754E-16,-1.));
#17003=DIRECTION('center_axis',(0.707106781186548,0.707106781186547,9.57563348951068E-17));
#17004=DIRECTION('ref_axis',(1.354199074918E-16,0.,-1.));
#17005=DIRECTION('',(0.,-1.354199074918E-16,1.));
#17006=DIRECTION('',(0.,1.354199074918E-16,-1.));
#17007=DIRECTION('center_axis',(0.,0.499999999999999,-0.866025403784439));
#17008=DIRECTION('ref_axis',(0.,-0.866025403784439,-0.499999999999999));
#17009=DIRECTION('',(-1.,0.,0.));
#17010=DIRECTION('',(-1.,0.,0.));
#17011=DIRECTION('center_axis',(0.,1.,-4.062597224754E-16));
#17012=DIRECTION('ref_axis',(0.,-4.062597224754E-16,-1.));
#17013=DIRECTION('',(-1.,0.,0.));
#17014=DIRECTION('center_axis',(0.,0.5,0.866025403784439));
#17015=DIRECTION('ref_axis',(0.,0.866025403784439,-0.5));
#17016=DIRECTION('',(-1.,0.,0.));
#17017=DIRECTION('center_axis',(1.,0.,0.));
#17018=DIRECTION('ref_axis',(0.,0.,-1.));
#17019=DIRECTION('',(0.,-1.,0.));
#17020=DIRECTION('center_axis',(-0.577350269189626,-0.577350269189625,0.577350269189627));
#17021=DIRECTION('ref_axis',(0.707106781186548,0.,0.707106781186547));
#17022=DIRECTION('',(0.707106781186548,7.8504622934189E-16,0.707106781186548));
#17023=DIRECTION('',(-0.707106781186547,0.707106781186548,0.));
#17024=DIRECTION('',(0.,-0.707106781186549,-0.707106781186546));
#17025=DIRECTION('center_axis',(-0.707106781186548,-0.707106781186547,0.));
#17026=DIRECTION('ref_axis',(0.,0.,1.));
#17027=DIRECTION('',(-0.707106781186547,0.707106781186548,0.));
#17028=DIRECTION('',(0.,0.,1.));
#17029=DIRECTION('',(0.,0.,-1.));
#17030=DIRECTION('center_axis',(0.577350269189625,-0.577350269189625,0.577350269189627));
#17031=DIRECTION('ref_axis',(0.707106781186549,0.,-0.707106781186546));
#17032=DIRECTION('',(0.,0.707106781186549,0.707106781186546));
#17033=DIRECTION('',(-0.707106781186548,-0.707106781186547,0.));
#17034=DIRECTION('',(0.707106781186549,0.,-0.707106781186546));
#17035=DIRECTION('center_axis',(0.707106781186547,-0.707106781186548,0.));
#17036=DIRECTION('ref_axis',(0.,0.,-1.));
#17037=DIRECTION('',(-0.707106781186548,-0.707106781186547,0.));
#17038=DIRECTION('',(0.,0.,1.));
#17039=DIRECTION('',(0.,0.,-1.));
#17040=DIRECTION('center_axis',(0.707106781186546,0.,0.707106781186549));
#17041=DIRECTION('ref_axis',(0.707106781186549,0.,-0.707106781186546));
#17042=DIRECTION('',(-0.577350269189628,-0.577350269189623,0.577350269189626));
#17043=DIRECTION('',(0.,-1.,0.));
#17044=DIRECTION('',(0.,1.,0.));
#17045=DIRECTION('',(-0.577350269189627,0.577350269189625,0.577350269189625));
#17046=DIRECTION('center_axis',(0.,-0.707106781186546,0.707106781186549));
#17047=DIRECTION('ref_axis',(1.,0.,0.));
#17048=DIRECTION('',(-1.,0.,0.));
#17049=DIRECTION('',(1.,0.,0.));
#17050=DIRECTION('center_axis',(-0.707106781186548,0.,0.707106781186548));
#17051=DIRECTION('ref_axis',(0.707106781186548,0.,0.707106781186548));
#17052=DIRECTION('',(-0.577350269189627,-0.577350269189624,-0.577350269189627));
#17053=DIRECTION('',(0.,-1.,0.));
#17054=DIRECTION('',(0.,1.,0.));
#17055=DIRECTION('',(-0.577350269189627,0.577350269189624,-0.577350269189627));
#17056=DIRECTION('center_axis',(0.,-1.,0.));
#17057=DIRECTION('ref_axis',(1.,0.,0.));
#17058=DIRECTION('',(-1.,0.,0.));
#17059=DIRECTION('center_axis',(-1.,0.,0.));
#17060=DIRECTION('ref_axis',(0.,-1.,0.));
#17061=DIRECTION('',(0.,0.,1.));
#17062=DIRECTION('',(0.,1.,0.));
#17063=DIRECTION('center_axis',(-0.707106781186546,0.707106781186549,0.));
#17064=DIRECTION('ref_axis',(0.,0.,1.));
#17065=DIRECTION('',(0.577350269189627,0.577350269189624,-0.577350269189627));
#17066=DIRECTION('',(0.,0.,-1.));
#17067=DIRECTION('',(0.577350269189625,0.577350269189622,-0.57735026918963));
#17068=DIRECTION('center_axis',(-0.577350269189625,-0.577350269189626,0.577350269189627));
#17069=DIRECTION('ref_axis',(0.707106781186549,0.,0.707106781186546));
#17070=DIRECTION('',(0.707106781186549,7.85046229341889E-16,0.707106781186546));
#17071=DIRECTION('',(-0.707106781186548,0.707106781186547,0.));
#17072=DIRECTION('',(7.85046229341889E-16,-0.707106781186549,-0.707106781186546));
#17073=DIRECTION('center_axis',(-0.707106781186547,-0.707106781186548,0.));
#17074=DIRECTION('ref_axis',(0.,0.,1.));
#17075=DIRECTION('',(-0.707106781186548,0.707106781186547,0.));
#17076=DIRECTION('',(0.,0.,1.));
#17077=DIRECTION('',(0.,0.,-1.));
#17078=DIRECTION('center_axis',(0.577350269189625,-0.577350269189626,0.577350269189627));
#17079=DIRECTION('ref_axis',(0.707106781186549,0.,-0.707106781186546));
#17080=DIRECTION('',(0.,0.707106781186549,0.707106781186546));
#17081=DIRECTION('',(-0.707106781186548,-0.707106781186547,0.));
#17082=DIRECTION('',(0.707106781186549,0.,-0.707106781186546));
#17083=DIRECTION('center_axis',(0.707106781186547,-0.707106781186548,0.));
#17084=DIRECTION('ref_axis',(0.,0.,-1.));
#17085=DIRECTION('',(-0.707106781186548,-0.707106781186547,0.));
#17086=DIRECTION('',(0.,0.,1.));
#17087=DIRECTION('',(0.,0.,-1.));
#17088=DIRECTION('center_axis',(0.707106781186546,0.,0.707106781186549));
#17089=DIRECTION('ref_axis',(0.707106781186549,0.,-0.707106781186546));
#17090=DIRECTION('',(-0.577350269189628,-0.577350269189623,0.577350269189626));
#17091=DIRECTION('',(0.,-1.,0.));
#17092=DIRECTION('',(0.,1.,0.));
#17093=DIRECTION('',(-0.577350269189628,0.577350269189624,0.577350269189626));
#17094=DIRECTION('center_axis',(0.,-0.707106781186546,0.707106781186549));
#17095=DIRECTION('ref_axis',(1.,0.,0.));
#17096=DIRECTION('',(-1.,0.,0.));
#17097=DIRECTION('',(1.,0.,0.));
#17098=DIRECTION('center_axis',(-0.707106781186546,0.,0.707106781186549));
#17099=DIRECTION('ref_axis',(0.707106781186549,0.,0.707106781186546));
#17100=DIRECTION('',(-0.577350269189626,-0.577350269189627,-0.577350269189624));
#17101=DIRECTION('',(0.,-1.,0.));
#17102=DIRECTION('',(0.,1.,0.));
#17103=DIRECTION('',(-0.577350269189628,0.577350269189623,-0.577350269189626));
#17104=DIRECTION('center_axis',(0.,-1.,0.));
#17105=DIRECTION('ref_axis',(1.,0.,0.));
#17106=DIRECTION('',(-1.,0.,0.));
#17107=DIRECTION('center_axis',(-1.,0.,0.));
#17108=DIRECTION('ref_axis',(0.,-1.,0.));
#17109=DIRECTION('',(0.,0.,1.));
#17110=DIRECTION('',(0.,1.,0.));
#17111=DIRECTION('center_axis',(-0.707106781186548,0.707106781186547,0.));
#17112=DIRECTION('ref_axis',(0.,0.,1.));
#17113=DIRECTION('',(0.577350269189624,0.577350269189625,-0.577350269189628));
#17114=DIRECTION('',(0.,0.,-1.));
#17115=DIRECTION('',(0.577350269189622,0.577350269189624,-0.577350269189631));
#17116=DIRECTION('center_axis',(-0.707106781186546,0.,0.707106781186549));
#17117=DIRECTION('ref_axis',(0.707106781186549,0.,0.707106781186546));
#17118=DIRECTION('',(0.,1.,0.));
#17119=DIRECTION('',(-0.577350269189628,0.577350269189623,-0.577350269189626));
#17120=DIRECTION('',(-0.577350269189627,-0.577350269189627,-0.577350269189624));
#17121=DIRECTION('',(0.,-1.,0.));
#17122=DIRECTION('center_axis',(-1.,0.,0.));
#17123=DIRECTION('ref_axis',(0.,-1.,0.));
#17124=DIRECTION('',(0.,0.,1.));
#17125=DIRECTION('',(0.,1.,0.));
#17126=DIRECTION('center_axis',(-0.707106781186548,0.707106781186548,0.));
#17127=DIRECTION('ref_axis',(0.,0.,1.));
#17128=DIRECTION('',(0.577350269189625,0.577350269189625,-0.577350269189627));
#17129=DIRECTION('',(0.,0.,-1.));
#17130=DIRECTION('',(0.577350269189623,0.577350269189623,-0.577350269189631));
#17131=DIRECTION('center_axis',(0.,0.707106781186552,0.707106781186543));
#17132=DIRECTION('ref_axis',(1.,0.,0.));
#17133=DIRECTION('',(1.,0.,0.));
#17134=DIRECTION('',(-0.577350269189618,-0.577350269189626,0.577350269189633));
#17135=DIRECTION('',(-1.,0.,0.));
#17136=DIRECTION('',(0.577350269189625,-0.577350269189622,0.57735026918963));
#17137=DIRECTION('center_axis',(0.707106781186546,0.707106781186549,0.));
#17138=DIRECTION('ref_axis',(0.,0.,-1.));
#17139=DIRECTION('',(0.,0.,1.));
#17140=DIRECTION('',(-0.577350269189625,0.577350269189622,0.57735026918963));
#17141=DIRECTION('',(0.,0.,-1.));
#17142=DIRECTION('center_axis',(0.,0.,-1.));
#17143=DIRECTION('ref_axis',(1.,0.,0.));
#17144=DIRECTION('',(0.,-1.,0.));
#17145=DIRECTION('',(1.,0.,0.));
#17146=DIRECTION('',(0.,-1.,0.));
#17147=DIRECTION('center_axis',(-1.,0.,0.));
#17148=DIRECTION('ref_axis',(0.,0.,-1.));
#17149=DIRECTION('',(0.,-1.,0.));
#17150=DIRECTION('',(0.,0.,-1.));
#17151=DIRECTION('center_axis',(-0.707106781186552,0.707106781186543,0.));
#17152=DIRECTION('ref_axis',(0.,0.,1.));
#17153=DIRECTION('',(0.,0.,-1.));
#17154=DIRECTION('',(0.,0.,1.));
#17155=DIRECTION('',(0.577350269189618,0.577350269189626,0.577350269189633));
#17156=DIRECTION('center_axis',(0.,0.707106781186552,-0.707106781186543));
#17157=DIRECTION('ref_axis',(-1.,0.,0.));
#17158=DIRECTION('',(-1.,0.,0.));
#17159=DIRECTION('',(1.,0.,0.));
#17160=DIRECTION('center_axis',(0.,1.,0.));
#17161=DIRECTION('ref_axis',(-1.,0.,0.));
#17162=DIRECTION('',(1.,0.,0.));
#17163=DIRECTION('',(0.,0.,-1.));
#17164=DIRECTION('center_axis',(0.,1.,0.));
#17165=DIRECTION('ref_axis',(1.,0.,0.));
#17166=DIRECTION('',(0.,0.,-1.));
#17167=DIRECTION('',(-1.,0.,0.));
#17168=DIRECTION('',(-1.,0.,0.));
#17169=DIRECTION('',(0.,0.,1.));
#17170=DIRECTION('',(-1.,0.,0.));
#17171=DIRECTION('',(-1.,0.,0.));
#17172=DIRECTION('',(0.,0.,1.));
#17173=DIRECTION('',(-1.,0.,0.));
#17174=DIRECTION('',(-1.,0.,0.));
#17175=DIRECTION('',(0.,0.,1.));
#17176=DIRECTION('',(-1.,0.,0.));
#17177=DIRECTION('',(0.,0.,1.));
#17178=DIRECTION('center_axis',(0.,1.,0.));
#17179=DIRECTION('ref_axis',(-1.,0.,0.));
#17180=DIRECTION('',(0.,0.,1.));
#17181=DIRECTION('center_axis',(0.,0.707106781186546,-0.707106781186549));
#17182=DIRECTION('ref_axis',(-1.,0.,0.));
#17183=DIRECTION('',(-6.28036983473511E-15,0.707106781186549,0.707106781186546));
#17184=DIRECTION('',(0.,-0.707106781186549,-0.707106781186546));
#17185=DIRECTION('',(-1.,0.,0.));
#17186=DIRECTION('center_axis',(0.,0.,1.));
#17187=DIRECTION('ref_axis',(-0.707106781186546,0.707106781186548,0.));
#17188=DIRECTION('',(-0.707106781186544,-1.57009245868379E-15,0.707106781186551));
#17189=DIRECTION('center_axis',(0.,0.,-1.));
#17190=DIRECTION('ref_axis',(-0.707106781186546,0.707106781186549,0.));
#17191=DIRECTION('center_axis',(0.,0.,1.));
#17192=DIRECTION('ref_axis',(-0.707106781186546,0.707106781186549,0.));
#17193=DIRECTION('center_axis',(-0.707106781186548,0.,-0.707106781186548));
#17194=DIRECTION('ref_axis',(-0.707106781186548,0.,0.707106781186548));
#17195=DIRECTION('',(-0.707106781186548,0.,0.707106781186548));
#17196=DIRECTION('',(0.,1.,0.));
#17197=DIRECTION('',(0.,-1.,0.));
#17198=DIRECTION('center_axis',(0.,0.,1.));
#17199=DIRECTION('ref_axis',(-0.707106781186549,-0.707106781186546,0.));
#17200=DIRECTION('',(0.,-0.707106781186549,0.707106781186546));
#17201=DIRECTION('center_axis',(0.,0.,-1.));
#17202=DIRECTION('ref_axis',(-0.707106781186549,-0.707106781186546,0.));
#17203=DIRECTION('center_axis',(0.,0.,1.));
#17204=DIRECTION('ref_axis',(-0.707106781186549,-0.707106781186546,0.));
#17205=DIRECTION('center_axis',(0.,-0.707106781186546,-0.707106781186549));
#17206=DIRECTION('ref_axis',(-1.,0.,0.));
#17207=DIRECTION('',(0.,-0.707106781186549,0.707106781186546));
#17208=DIRECTION('',(-1.,0.,0.));
#17209=DIRECTION('',(1.,0.,0.));
#17210=DIRECTION('center_axis',(0.,0.,1.));
#17211=DIRECTION('ref_axis',(0.707106781186549,-0.707106781186546,0.));
#17212=DIRECTION('',(0.707106781186554,0.,0.707106781186541));
#17213=DIRECTION('center_axis',(0.,0.,-1.));
#17214=DIRECTION('ref_axis',(0.707106781186549,-0.707106781186546,0.));
#17215=DIRECTION('center_axis',(0.,0.,1.));
#17216=DIRECTION('ref_axis',(0.707106781186549,-0.707106781186546,0.));
#17217=DIRECTION('center_axis',(0.707106781186548,0.,-0.707106781186548));
#17218=DIRECTION('ref_axis',(-0.707106781186548,0.,-0.707106781186548));
#17219=DIRECTION('',(0.707106781186548,0.,0.707106781186548));
#17220=DIRECTION('',(0.,-1.,0.));
#17221=DIRECTION('',(0.,1.,0.));
#17222=DIRECTION('center_axis',(0.,0.,1.));
#17223=DIRECTION('ref_axis',(0.707106781186548,0.707106781186547,0.));
#17224=DIRECTION('center_axis',(0.,0.,-1.));
#17225=DIRECTION('ref_axis',(0.707106781186548,0.707106781186547,0.));
#17226=DIRECTION('center_axis',(0.,0.,1.));
#17227=DIRECTION('ref_axis',(0.707106781186548,0.707106781186547,0.));
#17228=DIRECTION('center_axis',(0.,0.,1.));
#17229=DIRECTION('ref_axis',(0.707106781186549,-0.707106781186546,0.));
#17230=DIRECTION('',(0.,0.,1.));
#17231=DIRECTION('center_axis',(0.,0.,1.));
#17232=DIRECTION('ref_axis',(0.707106781186549,-0.707106781186546,0.));
#17233=DIRECTION('',(0.,0.,-1.));
#17234=DIRECTION('center_axis',(1.,0.,0.));
#17235=DIRECTION('ref_axis',(0.,1.,0.));
#17236=DIRECTION('',(0.,0.,-1.));
#17237=DIRECTION('',(0.,1.,0.));
#17238=DIRECTION('center_axis',(1.,0.,0.));
#17239=DIRECTION('ref_axis',(0.,0.,-1.));
#17240=DIRECTION('center_axis',(0.,0.,1.));
#17241=DIRECTION('ref_axis',(0.707106781186548,0.707106781186547,0.));
#17242=DIRECTION('center_axis',(0.,0.,1.));
#17243=DIRECTION('ref_axis',(0.707106781186548,0.707106781186547,0.));
#17244=DIRECTION('center_axis',(0.,0.,1.));
#17245=DIRECTION('ref_axis',(1.,0.,0.));
#17246=DIRECTION('center_axis',(0.,0.707106781186552,0.707106781186543));
#17247=DIRECTION('ref_axis',(1.,0.,0.));
#17248=DIRECTION('',(1.,0.,0.));
#17249=DIRECTION('',(0.577350269189626,-0.577350269189622,0.57735026918963));
#17250=DIRECTION('center_axis',(0.,0.707106781186552,0.707106781186543));
#17251=DIRECTION('ref_axis',(1.,0.,0.));
#17252=DIRECTION('',(0.577350269189625,-0.577350269189622,0.57735026918963));
#17253=DIRECTION('',(1.,0.,0.));
#17254=DIRECTION('center_axis',(0.707106781186546,0.707106781186549,0.));
#17255=DIRECTION('ref_axis',(0.,0.,-1.));
#17256=DIRECTION('',(0.,0.,-1.));
#17257=DIRECTION('',(0.577350269189627,-0.577350269189624,0.577350269189627));
#17258=DIRECTION('center_axis',(0.,0.707106781186552,0.707106781186543));
#17259=DIRECTION('ref_axis',(1.,0.,0.));
#17260=DIRECTION('',(6.28036983473505E-15,-0.707106781186543,0.707106781186552));
#17261=DIRECTION('',(1.,0.,0.));
#17262=DIRECTION('center_axis',(0.,0.,-1.));
#17263=DIRECTION('ref_axis',(-0.707106781186546,0.707106781186548,0.));
#17264=DIRECTION('center_axis',(0.,0.,1.));
#17265=DIRECTION('ref_axis',(-0.707106781186546,0.707106781186549,0.));
#17266=DIRECTION('',(0.707106781186544,1.57009245868379E-15,0.707106781186551));
#17267=DIRECTION('center_axis',(0.,0.,-1.));
#17268=DIRECTION('ref_axis',(-0.707106781186546,0.707106781186549,0.));
#17269=DIRECTION('center_axis',(-0.707106781186554,0.,0.707106781186541));
#17270=DIRECTION('ref_axis',(0.707106781186541,0.,0.707106781186554));
#17271=DIRECTION('',(0.707106781186541,0.,0.707106781186554));
#17272=DIRECTION('',(0.,1.,0.));
#17273=DIRECTION('',(0.,-1.,0.));
#17274=DIRECTION('center_axis',(0.,0.,-1.));
#17275=DIRECTION('ref_axis',(-0.707106781186549,-0.707106781186546,0.));
#17276=DIRECTION('center_axis',(0.,0.,1.));
#17277=DIRECTION('ref_axis',(-0.707106781186549,-0.707106781186546,0.));
#17278=DIRECTION('',(0.,0.707106781186549,0.707106781186546));
#17279=DIRECTION('center_axis',(0.,0.,-1.));
#17280=DIRECTION('ref_axis',(-0.707106781186549,-0.707106781186546,0.));
#17281=DIRECTION('center_axis',(0.,-0.707106781186552,0.707106781186543));
#17282=DIRECTION('ref_axis',(1.,0.,0.));
#17283=DIRECTION('',(0.,0.707106781186543,0.707106781186552));
#17284=DIRECTION('',(-1.,0.,0.));
#17285=DIRECTION('',(1.,0.,0.));
#17286=DIRECTION('center_axis',(0.,0.,-1.));
#17287=DIRECTION('ref_axis',(0.707106781186549,-0.707106781186546,0.));
#17288=DIRECTION('',(-0.707106781186554,0.,0.707106781186541));
#17289=DIRECTION('center_axis',(0.,0.,-1.));
#17290=DIRECTION('ref_axis',(0.707106781186549,-0.707106781186546,0.));
#17291=DIRECTION('center_axis',(0.707106781186554,0.,0.707106781186541));
#17292=DIRECTION('ref_axis',(0.707106781186541,0.,-0.707106781186554));
#17293=DIRECTION('',(-0.707106781186541,0.,0.707106781186554));
#17294=DIRECTION('',(0.,-1.,0.));
#17295=DIRECTION('center_axis',(0.,0.,-1.));
#17296=DIRECTION('ref_axis',(0.707106781186548,0.707106781186547,0.));
#17297=DIRECTION('',(0.,-0.70710678118655,0.707106781186545));
#17298=DIRECTION('center_axis',(0.,0.,-1.));
#17299=DIRECTION('ref_axis',(0.707106781186548,0.707106781186547,0.));
#17300=DIRECTION('center_axis',(0.,0.707106781186552,0.707106781186543));
#17301=DIRECTION('ref_axis',(1.,0.,0.));
#17302=DIRECTION('',(1.,0.,0.));
#17303=DIRECTION('',(0.577350269189622,-0.577350269189624,0.577350269189632));
#17304=DIRECTION('center_axis',(0.707106781186549,0.707106781186546,0.));
#17305=DIRECTION('ref_axis',(0.,0.,-1.));
#17306=DIRECTION('',(0.577350269189623,-0.577350269189626,0.577350269189628));
#17307=DIRECTION('center_axis',(0.,0.707106781186549,0.707106781186546));
#17308=DIRECTION('ref_axis',(1.,0.,0.));
#17309=DIRECTION('',(1.,0.,0.));
#17310=DIRECTION('center_axis',(0.,0.707106781186549,0.707106781186546));
#17311=DIRECTION('ref_axis',(1.,0.,0.));
#17312=DIRECTION('',(1.,0.,0.));
#17313=DIRECTION('center_axis',(0.707106781186545,0.70710678118655,0.));
#17314=DIRECTION('ref_axis',(0.,0.,-1.));
#17315=DIRECTION('',(0.,0.,-1.));
#17316=DIRECTION('',(0.577350269189628,-0.577350269189624,0.577350269189626));
#17317=DIRECTION('center_axis',(0.,0.707106781186549,0.707106781186546));
#17318=DIRECTION('ref_axis',(1.,0.,0.));
#17319=DIRECTION('',(1.,0.,0.));
#17320=DIRECTION('center_axis',(0.,-1.,0.));
#17321=DIRECTION('ref_axis',(1.,0.,0.));
#17322=DIRECTION('',(0.,0.,1.));
#17323=DIRECTION('center_axis',(0.,0.,1.));
#17324=DIRECTION('ref_axis',(-0.707106781186549,-0.707106781186546,0.));
#17325=DIRECTION('',(0.,0.,-1.));
#17326=DIRECTION('center_axis',(-1.,0.,0.));
#17327=DIRECTION('ref_axis',(0.,-1.,0.));
#17328=DIRECTION('',(0.,0.,1.));
#17329=DIRECTION('center_axis',(0.,0.,1.));
#17330=DIRECTION('ref_axis',(-0.707106781186547,0.707106781186548,0.));
#17331=DIRECTION('center_axis',(1.,0.,0.));
#17332=DIRECTION('ref_axis',(0.,1.,0.));
#17333=DIRECTION('',(0.,-1.,0.));
#17334=DIRECTION('center_axis',(0.,0.,1.));
#17335=DIRECTION('ref_axis',(1.,0.,0.));
#17336=DIRECTION('center_axis',(0.,0.,1.));
#17337=DIRECTION('ref_axis',(1.,0.,0.));
#17338=DIRECTION('',(0.,-1.,0.));
#17339=DIRECTION('center_axis',(1.,0.,0.));
#17340=DIRECTION('ref_axis',(0.,1.,0.));
#17341=DIRECTION('center_axis',(0.,0.,1.));
#17342=DIRECTION('ref_axis',(1.,0.,0.));
#17343=DIRECTION('',(0.730513754696385,0.650233639534332,0.208676467809204));
#17344=DIRECTION('',(-0.730513754696388,-0.650233639534325,0.208676467809214));
#17345=DIRECTION('center_axis',(0.,1.,0.));
#17346=DIRECTION('ref_axis',(-1.,0.,0.));
#17347=DIRECTION('',(-0.491046375823994,-0.70710678118655,-0.508796085667056));
#17348=DIRECTION('center_axis',(0.,-1.,0.));
#17349=DIRECTION('ref_axis',(-1.,0.,0.));
#17350=DIRECTION('center_axis',(0.,-1.,0.));
#17351=DIRECTION('ref_axis',(-1.,0.,0.));
#17352=DIRECTION('',(0.491046375823994,0.70710678118655,-0.508796085667056));
#17353=DIRECTION('center_axis',(0.,-1.,0.));
#17354=DIRECTION('ref_axis',(1.,0.,0.));
#17355=DIRECTION('',(0.,-1.,0.));
#17356=DIRECTION('center_axis',(0.,-1.,0.));
#17357=DIRECTION('ref_axis',(1.,0.,0.));
#17358=DIRECTION('',(-0.730513754696398,0.650233639534323,-0.208676467809188));
#17359=DIRECTION('',(0.730513754696391,-0.650233639534327,-0.208676467809201));
#17360=DIRECTION('center_axis',(0.,1.,0.));
#17361=DIRECTION('ref_axis',(1.,0.,0.));
#17362=DIRECTION('',(0.491046375823994,-0.70710678118655,0.508796085667056));
#17363=DIRECTION('center_axis',(0.,-1.,0.));
#17364=DIRECTION('ref_axis',(1.,0.,0.));
#17365=DIRECTION('',(-0.491046375823994,0.70710678118655,0.508796085667056));
#17366=DIRECTION('center_axis',(0.,-1.,0.));
#17367=DIRECTION('ref_axis',(1.,0.,0.));
#17368=DIRECTION('',(0.,-1.,0.));
#17369=DIRECTION('center_axis',(0.,-1.,0.));
#17370=DIRECTION('ref_axis',(1.,0.,0.));
#17371=DIRECTION('center_axis',(1.,0.,0.));
#17372=DIRECTION('ref_axis',(0.,0.,-1.));
#17373=DIRECTION('',(-0.707106781186547,8.65956056235493E-17,-0.707106781186547));
#17374=DIRECTION('center_axis',(-1.,0.,0.));
#17375=DIRECTION('ref_axis',(0.,0.,-1.));
#17376=DIRECTION('center_axis',(-1.,0.,0.));
#17377=DIRECTION('ref_axis',(0.,0.,-1.));
#17378=DIRECTION('',(-1.,0.,0.));
#17379=DIRECTION('center_axis',(1.,0.,0.));
#17380=DIRECTION('ref_axis',(0.,0.,-1.));
#17381=DIRECTION('center_axis',(-1.,0.,0.));
#17382=DIRECTION('ref_axis',(0.,0.,-1.));
#17383=DIRECTION('center_axis',(-1.,0.,0.));
#17384=DIRECTION('ref_axis',(0.,0.,-1.));
#17385=DIRECTION('',(0.707106781186547,-8.65956056235493E-17,-0.707106781186547));
#17386=DIRECTION('center_axis',(1.,0.,0.));
#17387=DIRECTION('ref_axis',(0.,0.,1.));
#17388=DIRECTION('',(0.,0.,1.));
#17389=DIRECTION('',(0.,-1.,0.));
#17390=DIRECTION('center_axis',(0.,1.,0.));
#17391=DIRECTION('ref_axis',(1.,0.,0.));
#17392=DIRECTION('center_axis',(0.,1.,0.));
#17393=DIRECTION('ref_axis',(1.,0.,0.));
#17394=DIRECTION('center_axis',(0.,-0.5,0.866025403784439));
#17395=DIRECTION('ref_axis',(0.,0.866025403784439,0.5));
#17396=DIRECTION('',(-1.,0.,0.));
#17397=DIRECTION('center_axis',(0.,-1.,-1.354199074918E-16));
#17398=DIRECTION('ref_axis',(0.,-1.354199074918E-16,1.));
#17399=DIRECTION('',(-1.,0.,0.));
#17400=DIRECTION('center_axis',(0.,-0.499999999999999,-0.866025403784439));
#17401=DIRECTION('ref_axis',(0.,-0.866025403784439,0.499999999999999));
#17402=DIRECTION('center_axis',(0.,-0.499999999999999,-0.866025403784439));
#17403=DIRECTION('ref_axis',(0.,0.866025403784439,-0.499999999999999));
#17404=DIRECTION('',(1.,0.,0.));
#17405=DIRECTION('center_axis',(0.,-1.,-1.354199074918E-16));
#17406=DIRECTION('ref_axis',(0.,1.354199074918E-16,-1.));
#17407=DIRECTION('',(1.,0.,0.));
#17408=DIRECTION('center_axis',(0.,-0.5,0.866025403784439));
#17409=DIRECTION('ref_axis',(0.,-0.866025403784439,-0.5));
#17410=DIRECTION('center_axis',(0.,0.,1.));
#17411=DIRECTION('ref_axis',(-1.,0.,0.));
#17412=DIRECTION('',(-1.,0.,0.));
#17413=DIRECTION('center_axis',(0.,-1.,0.));
#17414=DIRECTION('ref_axis',(0.,0.,-1.));
#17415=DIRECTION('center_axis',(0.,0.,1.));
#17416=DIRECTION('ref_axis',(1.,0.,0.));
#17417=DIRECTION('axis',(0.,0.,1.));
#17418=DIRECTION('refdir',(1.,0.,0.));
#17419=DIRECTION('center_axis',(0.,-1.,0.));
#17420=DIRECTION('ref_axis',(1.,0.,0.));
#17421=DIRECTION('center_axis',(0.,-1.,0.));
#17422=DIRECTION('ref_axis',(1.,0.,0.));
#17423=DIRECTION('',(0.707106781186547,0.707106781186547,8.65956056235493E-17));
#17424=DIRECTION('center_axis',(0.,1.,0.));
#17425=DIRECTION('ref_axis',(1.,0.,0.));
#17426=DIRECTION('center_axis',(0.,-1.,0.));
#17427=DIRECTION('ref_axis',(1.,0.,0.));
#17428=DIRECTION('center_axis',(0.,-1.,0.));
#17429=DIRECTION('ref_axis',(1.,0.,0.));
#17430=DIRECTION('',(0.,-1.,0.));
#17431=DIRECTION('center_axis',(0.,1.,0.));
#17432=DIRECTION('ref_axis',(1.,0.,0.));
#17433=DIRECTION('',(-1.,0.,0.));
#17434=DIRECTION('center_axis',(0.,1.,0.));
#17435=DIRECTION('ref_axis',(0.707106781186547,0.,-0.707106781186547));
#17436=DIRECTION('',(0.,0.,-1.));
#17437=DIRECTION('center_axis',(0.,1.,0.));
#17438=DIRECTION('ref_axis',(0.707106781186547,0.,0.707106781186547));
#17439=DIRECTION('',(1.,0.,0.));
#17440=DIRECTION('center_axis',(0.,1.,0.));
#17441=DIRECTION('ref_axis',(-0.707106781186545,0.,0.70710678118655));
#17442=DIRECTION('',(0.,0.,1.));
#17443=DIRECTION('center_axis',(0.,1.,0.));
#17444=DIRECTION('ref_axis',(-0.707106781186547,0.,-0.707106781186547));
#17445=DIRECTION('center_axis',(0.,1.,0.));
#17446=DIRECTION('ref_axis',(1.,0.,0.));
#17447=DIRECTION('center_axis',(0.,1.,0.));
#17448=DIRECTION('ref_axis',(1.,0.,0.));
#17449=DIRECTION('center_axis',(0.,1.,0.));
#17450=DIRECTION('ref_axis',(1.,0.,0.));
#17451=DIRECTION('center_axis',(0.,1.,0.));
#17452=DIRECTION('ref_axis',(1.,0.,0.));
#17453=DIRECTION('',(0.707106781186547,-0.707106781186547,-8.65956056235493E-17));
#17454=DIRECTION('center_axis',(0.,1.,0.));
#17455=DIRECTION('ref_axis',(0.,0.,1.));
#17456=DIRECTION('',(-1.,0.,0.));
#17457=DIRECTION('center_axis',(0.,-1.,0.));
#17458=DIRECTION('ref_axis',(0.707106781186547,0.,0.707106781186547));
#17459=DIRECTION('',(0.,0.,1.));
#17460=DIRECTION('center_axis',(0.,-1.,0.));
#17461=DIRECTION('ref_axis',(0.707106781186547,0.,-0.707106781186547));
#17462=DIRECTION('',(1.,0.,0.));
#17463=DIRECTION('center_axis',(0.,-1.,0.));
#17464=DIRECTION('ref_axis',(-0.707106781186548,0.,-0.707106781186548));
#17465=DIRECTION('',(0.,0.,-1.));
#17466=DIRECTION('center_axis',(0.,-1.,0.));
#17467=DIRECTION('ref_axis',(-0.707106781186545,0.,0.70710678118655));
#17468=DIRECTION('center_axis',(0.,-1.,0.));
#17469=DIRECTION('ref_axis',(1.,0.,0.));
#17470=DIRECTION('center_axis',(0.,-1.,0.));
#17471=DIRECTION('ref_axis',(1.,0.,0.));
#17472=DIRECTION('center_axis',(0.,-0.70710678118654,-0.707106781186555));
#17473=DIRECTION('ref_axis',(-1.,0.,0.));
#17474=DIRECTION('',(0.,-0.707106781186555,0.70710678118654));
#17475=DIRECTION('',(0.,0.707106781186555,-0.70710678118654));
#17476=DIRECTION('',(1.,0.,0.));
#17477=DIRECTION('center_axis',(0.,1.,0.));
#17478=DIRECTION('ref_axis',(0.707106781186548,0.,-0.707106781186548));
#17479=DIRECTION('center_axis',(0.,-1.,0.));
#17480=DIRECTION('ref_axis',(0.707106781186548,0.,-0.707106781186548));
#17481=DIRECTION('',(-0.70710678118654,-0.707106781186555,0.));
#17482=DIRECTION('center_axis',(0.707106781186555,-0.70710678118654,0.));
#17483=DIRECTION('ref_axis',(0.,0.,-1.));
#17484=DIRECTION('',(-0.70710678118654,-0.707106781186555,0.));
#17485=DIRECTION('',(0.,0.,1.));
#17486=DIRECTION('center_axis',(0.,1.,0.));
#17487=DIRECTION('ref_axis',(0.707106781186548,0.,0.707106781186548));
#17488=DIRECTION('center_axis',(0.,-1.,0.));
#17489=DIRECTION('ref_axis',(0.707106781186548,0.,0.707106781186548));
#17490=DIRECTION('',(0.,-0.707106781186555,-0.70710678118654));
#17491=DIRECTION('center_axis',(0.,-0.70710678118654,0.707106781186555));
#17492=DIRECTION('ref_axis',(1.,0.,0.));
#17493=DIRECTION('',(0.,-0.707106781186555,-0.70710678118654));
#17494=DIRECTION('',(-1.,0.,0.));
#17495=DIRECTION('center_axis',(0.,1.,0.));
#17496=DIRECTION('ref_axis',(-0.707106781186545,0.,0.70710678118655));
#17497=DIRECTION('center_axis',(0.,-1.,0.));
#17498=DIRECTION('ref_axis',(-0.707106781186545,0.,0.70710678118655));
#17499=DIRECTION('',(0.707106781186524,-0.707106781186571,0.));
#17500=DIRECTION('center_axis',(-0.707106781186555,-0.70710678118654,0.));
#17501=DIRECTION('ref_axis',(0.,0.,1.));
#17502=DIRECTION('',(0.70710678118654,-0.707106781186555,0.));
#17503=DIRECTION('',(0.,0.,-1.));
#17504=DIRECTION('center_axis',(0.,1.,0.));
#17505=DIRECTION('ref_axis',(-0.707106781186548,0.,-0.707106781186548));
#17506=DIRECTION('center_axis',(0.,-1.,0.));
#17507=DIRECTION('ref_axis',(-0.707106781186548,0.,-0.707106781186548));
#17508=DIRECTION('center_axis',(0.,1.,0.));
#17509=DIRECTION('ref_axis',(0.707106781186548,0.,0.707106781186548));
#17510=DIRECTION('',(0.,1.,0.));
#17511=DIRECTION('center_axis',(0.,1.,0.));
#17512=DIRECTION('ref_axis',(0.707106781186548,0.,0.707106781186548));
#17513=DIRECTION('',(0.,-1.,0.));
#17514=DIRECTION('center_axis',(1.,0.,0.));
#17515=DIRECTION('ref_axis',(0.,0.,-1.));
#17516=DIRECTION('',(0.,-1.,0.));
#17517=DIRECTION('',(0.,0.,-1.));
#17518=DIRECTION('center_axis',(0.,1.,0.));
#17519=DIRECTION('ref_axis',(0.707106781186548,0.,-0.707106781186548));
#17520=DIRECTION('',(0.,1.,0.));
#17521=DIRECTION('center_axis',(0.,1.,0.));
#17522=DIRECTION('ref_axis',(0.707106781186548,0.,-0.707106781186548));
#17523=DIRECTION('center_axis',(0.,0.,-1.));
#17524=DIRECTION('ref_axis',(-1.,0.,0.));
#17525=DIRECTION('',(0.,-1.,0.));
#17526=DIRECTION('',(-1.,0.,0.));
#17527=DIRECTION('center_axis',(0.,0.382683432365099,0.923879532511283));
#17528=DIRECTION('ref_axis',(1.,0.,0.));
#17529=DIRECTION('',(0.,0.923879532511284,-0.382683432365096));
#17530=DIRECTION('',(-1.,0.,0.));
#17531=DIRECTION('',(0.,-0.923879532511284,0.382683432365096));
#17532=DIRECTION('',(1.,0.,0.));
#17533=DIRECTION('center_axis',(0.,-1.,0.));
#17534=DIRECTION('ref_axis',(0.707106781186548,0.,0.707106781186548));
#17535=DIRECTION('',(-0.382683432365087,0.923879532511288,0.));
#17536=DIRECTION('center_axis',(0.,-1.,0.));
#17537=DIRECTION('ref_axis',(0.707106781186548,0.,0.707106781186548));
#17538=DIRECTION('center_axis',(0.923879532511283,0.382683432365099,0.));
#17539=DIRECTION('ref_axis',(0.,0.,-1.));
#17540=DIRECTION('',(-0.382683432365096,0.923879532511284,0.));
#17541=DIRECTION('',(0.,0.,1.));
#17542=DIRECTION('center_axis',(0.,-1.,0.));
#17543=DIRECTION('ref_axis',(0.707106781186548,0.,-0.707106781186548));
#17544=DIRECTION('',(0.,0.923879532511288,0.382683432365087));
#17545=DIRECTION('center_axis',(0.,-1.,0.));
#17546=DIRECTION('ref_axis',(0.707106781186548,0.,-0.707106781186548));
#17547=DIRECTION('center_axis',(0.,0.382683432365099,-0.923879532511283));
#17548=DIRECTION('ref_axis',(-1.,0.,0.));
#17549=DIRECTION('',(0.,0.923879532511284,0.382683432365096));
#17550=DIRECTION('',(1.,0.,0.));
#17551=DIRECTION('center_axis',(0.,-1.,0.));
#17552=DIRECTION('ref_axis',(-0.707106781186549,0.,-0.707106781186546));
#17553=DIRECTION('',(0.382683432365086,0.923879532511288,0.));
#17554=DIRECTION('center_axis',(0.,-1.,0.));
#17555=DIRECTION('ref_axis',(-0.707106781186551,0.,-0.707106781186544));
#17556=DIRECTION('center_axis',(0.,1.,0.));
#17557=DIRECTION('ref_axis',(-0.707106781186548,0.,-0.707106781186548));
#17558=DIRECTION('center_axis',(-0.923879532511287,0.38268343236509,0.));
#17559=DIRECTION('ref_axis',(0.,0.,1.));
#17560=DIRECTION('',(0.38268343236509,0.923879532511286,0.));
#17561=DIRECTION('',(0.,0.,-1.));
#17562=DIRECTION('',(0.,0.,1.));
#17563=DIRECTION('center_axis',(0.,-1.,0.));
#17564=DIRECTION('ref_axis',(-0.707106781186544,0.,0.707106781186551));
#17565=DIRECTION('center_axis',(0.,-1.,0.));
#17566=DIRECTION('ref_axis',(-0.707106781186543,0.,0.707106781186552));
#17567=DIRECTION('center_axis',(0.,1.,0.));
#17568=DIRECTION('ref_axis',(-0.707106781186545,0.,0.70710678118655));
#17569=DIRECTION('center_axis',(0.,-1.,0.));
#17570=DIRECTION('ref_axis',(-0.707106781186547,0.,-0.707106781186547));
#17571=DIRECTION('',(-0.707106781186546,-0.707106781186549,0.));
#17572=DIRECTION('center_axis',(0.,1.,0.));
#17573=DIRECTION('ref_axis',(-0.707106781186551,0.,-0.707106781186544));
#17574=DIRECTION('',(0.,-0.707106781186543,-0.707106781186552));
#17575=DIRECTION('center_axis',(-0.707106781186549,0.707106781186546,0.));
#17576=DIRECTION('ref_axis',(0.,0.,1.));
#17577=DIRECTION('',(-0.70710678118654,-0.707106781186555,0.));
#17578=DIRECTION('',(0.,0.,1.));
#17579=DIRECTION('center_axis',(0.,-1.,0.));
#17580=DIRECTION('ref_axis',(-0.707106781186545,0.,0.70710678118655));
#17581=DIRECTION('',(0.,-0.707106781186549,0.707106781186546));
#17582=DIRECTION('center_axis',(0.,1.,0.));
#17583=DIRECTION('ref_axis',(-0.707106781186546,0.,0.707106781186549));
#17584=DIRECTION('center_axis',(0.,0.707106781186546,0.707106781186549));
#17585=DIRECTION('ref_axis',(1.,0.,0.));
#17586=DIRECTION('',(0.,-0.707106781186543,0.707106781186552));
#17587=DIRECTION('',(1.,0.,0.));
#17588=DIRECTION('center_axis',(0.,0.,1.));
#17589=DIRECTION('ref_axis',(1.,0.,0.));
#17590=DIRECTION('',(0.,1.,0.));
#17591=DIRECTION('center_axis',(0.,0.923879532511283,0.382683432365099));
#17592=DIRECTION('ref_axis',(0.,-0.382683432365099,0.923879532511283));
#17593=DIRECTION('',(0.,-0.382683432365094,0.923879532511285));
#17594=DIRECTION('',(0.,0.382683432365104,-0.923879532511281));
#17595=DIRECTION('center_axis',(0.,-1.,0.));
#17596=DIRECTION('ref_axis',(-0.707106781186546,0.,0.70710678118655));
#17597=DIRECTION('',(-0.923879532511281,-0.382683432365103,0.));
#17598=DIRECTION('center_axis',(-0.38268343236511,0.923879532511278,0.));
#17599=DIRECTION('ref_axis',(0.,0.,1.));
#17600=DIRECTION('',(-0.923879532511276,-0.382683432365115,0.));
#17601=DIRECTION('center_axis',(0.,-1.,0.));
#17602=DIRECTION('ref_axis',(-0.70710678118655,0.,-0.707106781186545));
#17603=DIRECTION('',(0.,-0.382683432365102,-0.923879532511282));
#17604=DIRECTION('center_axis',(0.,0.923879532511283,-0.382683432365099));
#17605=DIRECTION('ref_axis',(0.,0.382683432365099,0.923879532511283));
#17606=DIRECTION('',(0.,-0.382683432365094,-0.923879532511285));
#17607=DIRECTION('',(-1.,0.,0.));
#17608=DIRECTION('center_axis',(0.,-1.,0.));
#17609=DIRECTION('ref_axis',(0.707106781186548,0.,-0.707106781186548));
#17610=DIRECTION('',(0.923879532511287,-0.382683432365089,0.));
#17611=DIRECTION('center_axis',(0.,1.,0.));
#17612=DIRECTION('ref_axis',(0.707106781186547,0.,-0.707106781186547));
#17613=DIRECTION('center_axis',(0.382683432365109,0.923879532511279,0.));
#17614=DIRECTION('ref_axis',(0.,0.,1.));
#17615=DIRECTION('',(0.923879532511275,-0.382683432365119,0.));
#17616=DIRECTION('',(0.,0.,-1.));
#17617=DIRECTION('center_axis',(0.,-1.,0.));
#17618=DIRECTION('ref_axis',(0.707106781186548,0.,0.707106781186548));
#17619=DIRECTION('center_axis',(0.,1.,0.));
#17620=DIRECTION('ref_axis',(0.707106781186547,0.,0.707106781186547));
#17621=DIRECTION('center_axis',(0.,-1.,0.));
#17622=DIRECTION('ref_axis',(0.707106781186547,0.,-0.707106781186547));
#17623=DIRECTION('',(0.,-0.707106781186549,-0.707106781186546));
#17624=DIRECTION('',(0.707106781186552,-0.707106781186543,0.));
#17625=DIRECTION('center_axis',(0.707106781186549,0.707106781186546,0.));
#17626=DIRECTION('ref_axis',(0.,0.,-1.));
#17627=DIRECTION('',(-0.707106781186552,0.707106781186543,0.));
#17628=DIRECTION('center_axis',(0.,-1.,0.));
#17629=DIRECTION('ref_axis',(0.707106781186547,0.,0.707106781186547));
#17630=DIRECTION('center_axis',(0.,0.707106781186546,-0.707106781186549));
#17631=DIRECTION('ref_axis',(-1.,0.,0.));
#17632=DIRECTION('center_axis',(0.,-1.,0.));
#17633=DIRECTION('ref_axis',(1.,0.,0.));
#17634=DIRECTION('',(0.,-1.,0.));
#17635=DIRECTION('center_axis',(0.,-1.,0.));
#17636=DIRECTION('ref_axis',(1.,0.,0.));
#17637=DIRECTION('',(0.,-1.,0.));
#17638=DIRECTION('center_axis',(0.,1.,0.));
#17639=DIRECTION('ref_axis',(-0.707106781186548,0.,-0.707106781186548));
#17640=DIRECTION('',(0.,1.,0.));
#17641=DIRECTION('center_axis',(0.,1.,0.));
#17642=DIRECTION('ref_axis',(-0.707106781186545,0.,0.70710678118655));
#17643=DIRECTION('',(0.,-1.,0.));
#17644=DIRECTION('center_axis',(-1.,0.,0.));
#17645=DIRECTION('ref_axis',(0.,0.,1.));
#17646=DIRECTION('axis',(0.,0.,1.));
#17647=DIRECTION('refdir',(1.,0.,0.));
#17648=DIRECTION('center_axis',(-1.,0.,0.));
#17649=DIRECTION('ref_axis',(0.,0.,1.));
#17650=DIRECTION('',(0.,0.,-1.));
#17651=DIRECTION('',(0.,1.,0.));
#17652=DIRECTION('',(0.,0.,1.));
#17653=DIRECTION('',(0.,1.,0.));
#17654=DIRECTION('center_axis',(0.,0.,-1.));
#17655=DIRECTION('ref_axis',(-1.,0.,0.));
#17656=DIRECTION('',(1.,0.,0.));
#17657=DIRECTION('',(-1.,0.,0.));
#17658=DIRECTION('',(0.,1.,0.));
#17659=DIRECTION('center_axis',(1.,0.,0.));
#17660=DIRECTION('ref_axis',(0.,0.,-1.));
#17661=DIRECTION('',(0.,0.,1.));
#17662=DIRECTION('',(0.,0.,-1.));
#17663=DIRECTION('',(0.,1.,0.));
#17664=DIRECTION('center_axis',(0.,0.,1.));
#17665=DIRECTION('ref_axis',(1.,0.,0.));
#17666=DIRECTION('',(-1.,0.,0.));
#17667=DIRECTION('',(1.,0.,0.));
#17668=DIRECTION('center_axis',(0.,1.,0.));
#17669=DIRECTION('ref_axis',(0.,0.,1.));
#17670=DIRECTION('center_axis',(-1.,0.,0.));
#17671=DIRECTION('ref_axis',(0.,0.,1.));
#17672=DIRECTION('',(0.,0.,-1.));
#17673=DIRECTION('',(0.,1.,0.));
#17674=DIRECTION('',(0.,0.,1.));
#17675=DIRECTION('',(0.,1.,0.));
#17676=DIRECTION('center_axis',(0.,0.,-1.));
#17677=DIRECTION('ref_axis',(-1.,0.,0.));
#17678=DIRECTION('',(1.,0.,0.));
#17679=DIRECTION('',(-1.,0.,0.));
#17680=DIRECTION('',(0.,1.,0.));
#17681=DIRECTION('center_axis',(1.,0.,0.));
#17682=DIRECTION('ref_axis',(0.,0.,-1.));
#17683=DIRECTION('',(0.,0.,1.));
#17684=DIRECTION('',(0.,0.,-1.));
#17685=DIRECTION('',(0.,1.,0.));
#17686=DIRECTION('center_axis',(0.,0.,1.));
#17687=DIRECTION('ref_axis',(1.,0.,0.));
#17688=DIRECTION('',(-1.,0.,0.));
#17689=DIRECTION('',(1.,0.,0.));
#17690=DIRECTION('center_axis',(0.,1.,0.));
#17691=DIRECTION('ref_axis',(0.,0.,1.));
#17692=DIRECTION('center_axis',(-1.,0.,0.));
#17693=DIRECTION('ref_axis',(0.,0.,1.));
#17694=DIRECTION('',(0.,0.,-1.));
#17695=DIRECTION('',(0.,1.,0.));
#17696=DIRECTION('',(0.,0.,1.));
#17697=DIRECTION('',(0.,1.,0.));
#17698=DIRECTION('center_axis',(0.,0.,-1.));
#17699=DIRECTION('ref_axis',(-1.,0.,0.));
#17700=DIRECTION('',(1.,0.,0.));
#17701=DIRECTION('',(-1.,0.,0.));
#17702=DIRECTION('',(0.,1.,0.));
#17703=DIRECTION('center_axis',(1.,0.,0.));
#17704=DIRECTION('ref_axis',(0.,0.,-1.));
#17705=DIRECTION('',(0.,0.,1.));
#17706=DIRECTION('',(0.,0.,-1.));
#17707=DIRECTION('',(0.,1.,0.));
#17708=DIRECTION('center_axis',(0.,0.,1.));
#17709=DIRECTION('ref_axis',(1.,0.,0.));
#17710=DIRECTION('',(-1.,0.,0.));
#17711=DIRECTION('',(1.,0.,0.));
#17712=DIRECTION('center_axis',(0.,1.,0.));
#17713=DIRECTION('ref_axis',(0.,0.,1.));
#17714=DIRECTION('center_axis',(-1.,0.,0.));
#17715=DIRECTION('ref_axis',(0.,0.,1.));
#17716=DIRECTION('',(0.,0.,-1.));
#17717=DIRECTION('',(0.,1.,0.));
#17718=DIRECTION('',(0.,0.,1.));
#17719=DIRECTION('',(0.,1.,0.));
#17720=DIRECTION('center_axis',(0.,0.,-1.));
#17721=DIRECTION('ref_axis',(-1.,0.,0.));
#17722=DIRECTION('',(1.,0.,0.));
#17723=DIRECTION('',(-1.,0.,0.));
#17724=DIRECTION('',(0.,1.,0.));
#17725=DIRECTION('center_axis',(1.,0.,0.));
#17726=DIRECTION('ref_axis',(0.,0.,-1.));
#17727=DIRECTION('',(0.,0.,1.));
#17728=DIRECTION('',(0.,0.,-1.));
#17729=DIRECTION('',(0.,1.,0.));
#17730=DIRECTION('center_axis',(0.,0.,1.));
#17731=DIRECTION('ref_axis',(1.,0.,0.));
#17732=DIRECTION('',(-1.,0.,0.));
#17733=DIRECTION('',(1.,0.,0.));
#17734=DIRECTION('center_axis',(0.,1.,0.));
#17735=DIRECTION('ref_axis',(0.,0.,1.));
#17736=DIRECTION('center_axis',(0.,1.,0.));
#17737=DIRECTION('ref_axis',(1.,0.,0.));
#17738=DIRECTION('axis',(0.,0.,1.));
#17739=DIRECTION('refdir',(1.,0.,0.));
#17740=DIRECTION('center_axis',(0.577350269189623,0.577350269189625,-0.57735026918963));
#17741=DIRECTION('ref_axis',(-0.707106781186552,0.,-0.707106781186544));
#17742=DIRECTION('',(-0.707106781186548,0.707106781186546,0.));
#17743=DIRECTION('',(0.707106781186552,0.,0.707106781186543));
#17744=DIRECTION('',(0.,-0.70710678118655,-0.707106781186544));
#17745=DIRECTION('center_axis',(0.577350269189623,0.577350269189625,0.57735026918963));
#17746=DIRECTION('ref_axis',(0.707106781186552,0.,-0.707106781186543));
#17747=DIRECTION('',(0.,0.70710678118655,-0.707106781186544));
#17748=DIRECTION('',(-0.707106781186552,0.,0.707106781186543));
#17749=DIRECTION('',(0.707106781186548,-0.707106781186546,0.));
#17750=DIRECTION('center_axis',(0.577350269189624,-0.577350269189624,-0.57735026918963));
#17751=DIRECTION('ref_axis',(-0.707106781186552,0.,-0.707106781186544));
#17752=DIRECTION('',(-0.707106781186552,0.,-0.707106781186543));
#17753=DIRECTION('',(0.707106781186547,0.707106781186547,0.));
#17754=DIRECTION('',(0.,-0.707106781186552,0.707106781186543));
#17755=DIRECTION('center_axis',(-0.577350269189625,0.577350269189624,-0.577350269189629));
#17756=DIRECTION('ref_axis',(-0.70710678118655,0.,0.707106781186545));
#17757=DIRECTION('',(0.,0.70710678118655,0.707106781186544));
#17758=DIRECTION('',(0.70710678118655,0.,-0.707106781186545));
#17759=DIRECTION('',(-0.707106781186546,-0.707106781186549,0.));
#17760=DIRECTION('center_axis',(0.577350269189624,-0.577350269189624,0.57735026918963));
#17761=DIRECTION('ref_axis',(0.707106781186552,0.,-0.707106781186544));
#17762=DIRECTION('',(0.707106781186552,0.,-0.707106781186543));
#17763=DIRECTION('',(0.,0.707106781186552,0.707106781186543));
#17764=DIRECTION('',(-0.707106781186547,-0.707106781186547,0.));
#17765=DIRECTION('center_axis',(-0.577350269189626,0.577350269189625,0.577350269189626));
#17766=DIRECTION('ref_axis',(0.707106781186547,0.,0.707106781186547));
#17767=DIRECTION('',(0.707106781186546,0.707106781186549,0.));
#17768=DIRECTION('',(-0.707106781186547,0.,-0.707106781186547));
#17769=DIRECTION('',(-4.02587809918918E-15,-0.70710678118655,0.707106781186544));
#17770=DIRECTION('center_axis',(-0.577350269189626,-0.577350269189623,-0.577350269189629));
#17771=DIRECTION('ref_axis',(-0.70710678118655,0.,0.707106781186545));
#17772=DIRECTION('',(-0.70710678118655,0.,0.707106781186545));
#17773=DIRECTION('',(0.,0.707106781186552,-0.707106781186543));
#17774=DIRECTION('',(0.707106781186545,-0.70710678118655,0.));
#17775=DIRECTION('center_axis',(0.,-0.707106781186543,-0.707106781186552));
#17776=DIRECTION('ref_axis',(-1.,0.,0.));
#17777=DIRECTION('',(-1.,0.,0.));
#17778=DIRECTION('',(1.,0.,0.));
#17779=DIRECTION('center_axis',(-0.577350269189627,-0.577350269189624,0.577350269189627));
#17780=DIRECTION('ref_axis',(0.707106781186547,0.,0.707106781186547));
#17781=DIRECTION('',(-0.707106781186545,0.70710678118655,0.));
#17782=DIRECTION('',(4.02587809918917E-15,-0.707106781186552,-0.707106781186543));
#17783=DIRECTION('',(0.707106781186547,0.,0.707106781186547));
#17784=DIRECTION('center_axis',(0.,-0.707106781186543,0.707106781186552));
#17785=DIRECTION('ref_axis',(1.,0.,0.));
#17786=DIRECTION('',(1.,0.,0.));
#17787=DIRECTION('',(-1.,0.,0.));
#17788=DIRECTION('center_axis',(-0.707106781186548,0.,0.707106781186548));
#17789=DIRECTION('ref_axis',(0.707106781186548,0.,0.707106781186548));
#17790=DIRECTION('',(0.,-1.,0.));
#17791=DIRECTION('',(0.,1.,0.));
#17792=DIRECTION('center_axis',(-0.70710678118655,-0.707106781186546,0.));
#17793=DIRECTION('ref_axis',(0.,0.,1.));
#17794=DIRECTION('',(0.,0.,1.));
#17795=DIRECTION('',(0.,0.,-1.));
#17796=DIRECTION('center_axis',(-0.707106781186545,0.,-0.70710678118655));
#17797=DIRECTION('ref_axis',(-0.70710678118655,0.,0.707106781186545));
#17798=DIRECTION('',(0.,-1.,0.));
#17799=DIRECTION('',(0.,1.,0.));
#17800=DIRECTION('center_axis',(0.,0.707106781186545,0.707106781186551));
#17801=DIRECTION('ref_axis',(1.,0.,0.));
#17802=DIRECTION('',(-1.,0.,0.));
#17803=DIRECTION('',(1.,0.,0.));
#17804=DIRECTION('center_axis',(-0.707106781186549,0.707106781186546,0.));
#17805=DIRECTION('ref_axis',(0.,0.,1.));
#17806=DIRECTION('',(0.,0.,-1.));
#17807=DIRECTION('',(0.,0.,1.));
#17808=DIRECTION('center_axis',(0.707106781186548,-0.707106781186548,0.));
#17809=DIRECTION('ref_axis',(0.,0.,-1.));
#17810=DIRECTION('',(0.,0.,-1.));
#17811=DIRECTION('',(0.,0.,1.));
#17812=DIRECTION('center_axis',(0.707106781186543,0.,0.707106781186552));
#17813=DIRECTION('ref_axis',(0.707106781186552,0.,-0.707106781186543));
#17814=DIRECTION('',(0.,-1.,0.));
#17815=DIRECTION('',(0.,1.,0.));
#17816=DIRECTION('center_axis',(0.,0.707106781186545,-0.707106781186551));
#17817=DIRECTION('ref_axis',(-1.,0.,0.));
#17818=DIRECTION('',(1.,0.,0.));
#17819=DIRECTION('',(-1.,0.,0.));
#17820=DIRECTION('center_axis',(0.707106781186543,0.,-0.707106781186552));
#17821=DIRECTION('ref_axis',(-0.707106781186552,0.,-0.707106781186543));
#17822=DIRECTION('',(0.,-1.,0.));
#17823=DIRECTION('',(0.,1.,0.));
#17824=DIRECTION('center_axis',(0.707106781186547,0.707106781186549,0.));
#17825=DIRECTION('ref_axis',(0.,0.,-1.));
#17826=DIRECTION('',(0.,0.,1.));
#17827=DIRECTION('',(0.,0.,-1.));
#17828=DIRECTION('center_axis',(0.,0.,-1.));
#17829=DIRECTION('ref_axis',(-1.,0.,0.));
#17830=DIRECTION('center_axis',(0.,0.,1.));
#17831=DIRECTION('ref_axis',(1.,0.,0.));
#17832=DIRECTION('center_axis',(0.,1.,0.));
#17833=DIRECTION('ref_axis',(1.,0.,0.));
#17834=DIRECTION('center_axis',(0.,1.,0.));
#17835=DIRECTION('ref_axis',(1.,0.,0.));
#17836=DIRECTION('center_axis',(-1.,0.,0.));
#17837=DIRECTION('ref_axis',(0.,0.,1.));
#17838=DIRECTION('center_axis',(0.,1.,0.));
#17839=DIRECTION('ref_axis',(0.,0.,1.));
#17840=DIRECTION('center_axis',(0.,-1.,0.));
#17841=DIRECTION('ref_axis',(1.,0.,0.));
#17842=DIRECTION('center_axis',(1.,0.,0.));
#17843=DIRECTION('ref_axis',(0.,0.,-1.));
#17844=DIRECTION('center_axis',(0.,-1.,0.));
#17845=DIRECTION('ref_axis',(1.,0.,0.));
#17846=DIRECTION('',(0.,-1.,0.));
#17847=DIRECTION('axis',(0.,0.,1.));
#17848=DIRECTION('refdir',(1.,0.,0.));
#17849=DIRECTION('center_axis',(1.,0.,0.));
#17850=DIRECTION('ref_axis',(0.,1.,0.));
#17851=DIRECTION('',(-1.,0.,0.));
#17852=DIRECTION('center_axis',(1.,0.,0.));
#17853=DIRECTION('ref_axis',(0.,1.,0.));
#17854=DIRECTION('center_axis',(1.,0.,0.));
#17855=DIRECTION('ref_axis',(0.,1.,0.));
#17856=DIRECTION('',(-1.,0.,0.));
#17857=DIRECTION('center_axis',(1.,0.,0.));
#17858=DIRECTION('ref_axis',(0.,1.,0.));
#17859=DIRECTION('',(-1.,0.,0.));
#17860=DIRECTION('center_axis',(1.,0.,0.));
#17861=DIRECTION('ref_axis',(0.,1.,0.));
#17862=DIRECTION('',(-1.,0.,0.));
#17863=DIRECTION('center_axis',(1.,0.,0.));
#17864=DIRECTION('ref_axis',(0.,1.,0.));
#17865=DIRECTION('',(-1.,0.,0.));
#17866=DIRECTION('center_axis',(1.,0.,0.));
#17867=DIRECTION('ref_axis',(0.,1.,0.));
#17868=DIRECTION('',(-1.,0.,0.));
#17869=DIRECTION('center_axis',(1.,0.,0.));
#17870=DIRECTION('ref_axis',(0.,1.,0.));
#17871=DIRECTION('',(-1.,0.,0.));
#17872=DIRECTION('center_axis',(1.,0.,0.));
#17873=DIRECTION('ref_axis',(0.,1.,0.));
#17874=DIRECTION('',(-1.,0.,0.));
#17875=DIRECTION('center_axis',(1.,0.,0.));
#17876=DIRECTION('ref_axis',(0.,1.,0.));
#17877=DIRECTION('',(-1.,0.,0.));
#17878=DIRECTION('center_axis',(1.,0.,0.));
#17879=DIRECTION('ref_axis',(0.,1.,0.));
#17880=DIRECTION('',(-1.,0.,0.));
#17881=DIRECTION('center_axis',(1.,0.,0.));
#17882=DIRECTION('ref_axis',(0.,1.,0.));
#17883=DIRECTION('',(-1.,0.,0.));
#17884=DIRECTION('center_axis',(1.,0.,0.));
#17885=DIRECTION('ref_axis',(0.,1.,0.));
#17886=DIRECTION('',(-1.,0.,0.));
#17887=DIRECTION('center_axis',(1.,0.,0.));
#17888=DIRECTION('ref_axis',(0.,1.,0.));
#17889=DIRECTION('',(-1.,0.,0.));
#17890=DIRECTION('center_axis',(1.,0.,0.));
#17891=DIRECTION('ref_axis',(0.,1.,0.));
#17892=DIRECTION('',(-1.,0.,0.));
#17893=DIRECTION('center_axis',(1.,0.,0.));
#17894=DIRECTION('ref_axis',(0.,1.,0.));
#17895=DIRECTION('',(-1.,0.,0.));
#17896=DIRECTION('center_axis',(1.,0.,0.));
#17897=DIRECTION('ref_axis',(0.,1.,0.));
#17898=DIRECTION('',(-1.,0.,0.));
#17899=DIRECTION('center_axis',(1.,0.,0.));
#17900=DIRECTION('ref_axis',(0.,1.,0.));
#17901=DIRECTION('',(-1.,0.,0.));
#17902=DIRECTION('center_axis',(1.,0.,0.));
#17903=DIRECTION('ref_axis',(0.,1.,0.));
#17904=DIRECTION('',(-1.,0.,0.));
#17905=DIRECTION('center_axis',(1.,0.,0.));
#17906=DIRECTION('ref_axis',(0.,1.,0.));
#17907=DIRECTION('',(-1.,0.,0.));
#17908=DIRECTION('center_axis',(1.,0.,0.));
#17909=DIRECTION('ref_axis',(0.,1.,0.));
#17910=DIRECTION('',(-1.,0.,0.));
#17911=DIRECTION('center_axis',(1.,0.,0.));
#17912=DIRECTION('ref_axis',(0.,1.,0.));
#17913=DIRECTION('',(-1.,0.,0.));
#17914=DIRECTION('center_axis',(1.,0.,0.));
#17915=DIRECTION('ref_axis',(0.,1.,0.));
#17916=DIRECTION('',(-1.,0.,0.));
#17917=DIRECTION('center_axis',(1.,0.,0.));
#17918=DIRECTION('ref_axis',(0.,1.,0.));
#17919=DIRECTION('',(-1.,0.,0.));
#17920=DIRECTION('center_axis',(1.,0.,0.));
#17921=DIRECTION('ref_axis',(0.,1.,0.));
#17922=DIRECTION('',(-1.,0.,0.));
#17923=DIRECTION('center_axis',(1.,0.,0.));
#17924=DIRECTION('ref_axis',(0.,1.,0.));
#17925=DIRECTION('',(-1.,0.,0.));
#17926=DIRECTION('center_axis',(1.,0.,0.));
#17927=DIRECTION('ref_axis',(0.,1.,0.));
#17928=DIRECTION('',(-1.,0.,0.));
#17929=DIRECTION('center_axis',(1.,0.,0.));
#17930=DIRECTION('ref_axis',(0.,1.,0.));
#17931=DIRECTION('',(-1.,0.,0.));
#17932=DIRECTION('center_axis',(1.,0.,0.));
#17933=DIRECTION('ref_axis',(0.,1.,0.));
#17934=DIRECTION('',(-1.,0.,0.));
#17935=DIRECTION('center_axis',(1.,0.,0.));
#17936=DIRECTION('ref_axis',(0.,0.925734886529886,-0.378173134769644));
#17937=DIRECTION('',(1.,0.,0.));
#17938=DIRECTION('center_axis',(1.,0.,0.));
#17939=DIRECTION('ref_axis',(0.,1.,-9.1414668091865E-14));
#17940=DIRECTION('center_axis',(1.,0.,0.));
#17941=DIRECTION('ref_axis',(0.,1.,-9.1414668091865E-14));
#17942=DIRECTION('',(1.,0.,0.));
#17943=DIRECTION('center_axis',(1.,0.,0.));
#17944=DIRECTION('ref_axis',(0.,1.,-9.1414668091865E-14));
#17945=DIRECTION('',(1.,0.,0.));
#17946=DIRECTION('center_axis',(1.,0.,0.));
#17947=DIRECTION('ref_axis',(0.,1.,-9.1414668091865E-14));
#17948=DIRECTION('',(1.,0.,0.));
#17949=DIRECTION('center_axis',(1.,0.,0.));
#17950=DIRECTION('ref_axis',(0.,1.,-9.1414668091865E-14));
#17951=DIRECTION('',(1.,0.,0.));
#17952=DIRECTION('center_axis',(1.,0.,0.));
#17953=DIRECTION('ref_axis',(0.,1.,-9.1414668091865E-14));
#17954=DIRECTION('',(1.,0.,0.));
#17955=DIRECTION('center_axis',(1.,0.,0.));
#17956=DIRECTION('ref_axis',(0.,1.,-9.1414668091865E-14));
#17957=DIRECTION('',(1.,0.,0.));
#17958=DIRECTION('center_axis',(1.,0.,0.));
#17959=DIRECTION('ref_axis',(0.,1.,-9.1414668091865E-14));
#17960=DIRECTION('',(1.,0.,0.));
#17961=DIRECTION('center_axis',(1.,0.,0.));
#17962=DIRECTION('ref_axis',(0.,1.,-9.1414668091865E-14));
#17963=DIRECTION('',(1.,0.,0.));
#17964=DIRECTION('center_axis',(1.,0.,0.));
#17965=DIRECTION('ref_axis',(0.,1.,-9.1414668091865E-14));
#17966=DIRECTION('',(1.,0.,0.));
#17967=DIRECTION('center_axis',(1.,0.,0.));
#17968=DIRECTION('ref_axis',(0.,1.,-9.1414668091865E-14));
#17969=DIRECTION('',(1.,0.,0.));
#17970=DIRECTION('center_axis',(1.,0.,0.));
#17971=DIRECTION('ref_axis',(0.,1.,-9.1414668091865E-14));
#17972=DIRECTION('',(1.,0.,0.));
#17973=DIRECTION('center_axis',(1.,0.,0.));
#17974=DIRECTION('ref_axis',(0.,1.,-9.1414668091865E-14));
#17975=DIRECTION('',(1.,0.,0.));
#17976=DIRECTION('center_axis',(1.,0.,0.));
#17977=DIRECTION('ref_axis',(0.,1.,-9.1414668091865E-14));
#17978=DIRECTION('',(1.,0.,0.));
#17979=DIRECTION('center_axis',(1.,0.,0.));
#17980=DIRECTION('ref_axis',(0.,1.,-9.1414668091865E-14));
#17981=DIRECTION('',(1.,0.,0.));
#17982=DIRECTION('center_axis',(1.,0.,0.));
#17983=DIRECTION('ref_axis',(0.,1.,-9.1414668091865E-14));
#17984=DIRECTION('',(1.,0.,0.));
#17985=DIRECTION('center_axis',(1.,0.,0.));
#17986=DIRECTION('ref_axis',(0.,1.,-9.1414668091865E-14));
#17987=DIRECTION('',(1.,0.,0.));
#17988=DIRECTION('center_axis',(1.,0.,0.));
#17989=DIRECTION('ref_axis',(0.,1.,-9.1414668091865E-14));
#17990=DIRECTION('',(1.,0.,0.));
#17991=DIRECTION('center_axis',(1.,0.,0.));
#17992=DIRECTION('ref_axis',(0.,1.,-9.1414668091865E-14));
#17993=DIRECTION('',(1.,0.,0.));
#17994=DIRECTION('center_axis',(1.,0.,0.));
#17995=DIRECTION('ref_axis',(0.,1.,-9.1414668091865E-14));
#17996=DIRECTION('',(1.,0.,0.));
#17997=DIRECTION('center_axis',(1.,0.,0.));
#17998=DIRECTION('ref_axis',(0.,1.,-9.1414668091865E-14));
#17999=DIRECTION('',(1.,0.,0.));
#18000=DIRECTION('center_axis',(1.,0.,0.));
#18001=DIRECTION('ref_axis',(0.,1.,-9.1414668091865E-14));
#18002=DIRECTION('',(1.,0.,0.));
#18003=DIRECTION('center_axis',(1.,0.,0.));
#18004=DIRECTION('ref_axis',(0.,1.,-9.1414668091865E-14));
#18005=DIRECTION('',(1.,0.,0.));
#18006=DIRECTION('center_axis',(1.,0.,0.));
#18007=DIRECTION('ref_axis',(0.,1.,-9.1414668091865E-14));
#18008=DIRECTION('',(1.,0.,0.));
#18009=DIRECTION('center_axis',(1.,0.,0.));
#18010=DIRECTION('ref_axis',(0.,1.,-9.1414668091865E-14));
#18011=DIRECTION('',(1.,0.,0.));
#18012=DIRECTION('center_axis',(1.,0.,0.));
#18013=DIRECTION('ref_axis',(0.,1.,-9.1414668091865E-14));
#18014=DIRECTION('',(1.,0.,0.));
#18015=DIRECTION('center_axis',(1.,0.,0.));
#18016=DIRECTION('ref_axis',(0.,1.,-9.1414668091865E-14));
#18017=DIRECTION('',(1.,0.,0.));
#18018=DIRECTION('center_axis',(1.,0.,0.));
#18019=DIRECTION('ref_axis',(0.,-1.,0.));
#18020=DIRECTION('center_axis',(-1.,0.,0.));
#18021=DIRECTION('ref_axis',(0.,1.,0.));
#18022=DIRECTION('',(-0.707106781186547,-0.707106781186547,-8.65956056235493E-17));
#18023=DIRECTION('center_axis',(1.,0.,0.));
#18024=DIRECTION('ref_axis',(0.,-1.,0.));
#18025=DIRECTION('center_axis',(-1.,0.,0.));
#18026=DIRECTION('ref_axis',(0.,1.,0.));
#18027=DIRECTION('center_axis',(-1.,0.,0.));
#18028=DIRECTION('ref_axis',(0.,-1.,0.));
#18029=DIRECTION('center_axis',(-1.,0.,0.));
#18030=DIRECTION('ref_axis',(0.,1.,0.));
#18031=DIRECTION('center_axis',(-1.,0.,0.));
#18032=DIRECTION('ref_axis',(0.,-1.,0.));
#18033=DIRECTION('center_axis',(-1.,0.,0.));
#18034=DIRECTION('ref_axis',(0.,1.,0.));
#18035=DIRECTION('center_axis',(-1.,0.,0.));
#18036=DIRECTION('ref_axis',(0.,-1.,0.));
#18037=DIRECTION('center_axis',(-1.,0.,0.));
#18038=DIRECTION('ref_axis',(0.,1.,0.));
#18039=DIRECTION('center_axis',(-1.,0.,0.));
#18040=DIRECTION('ref_axis',(0.,-1.,0.));
#18041=DIRECTION('center_axis',(-1.,0.,0.));
#18042=DIRECTION('ref_axis',(0.,1.,0.));
#18043=DIRECTION('center_axis',(-1.,0.,0.));
#18044=DIRECTION('ref_axis',(0.,-1.,0.));
#18045=DIRECTION('center_axis',(-1.,0.,0.));
#18046=DIRECTION('ref_axis',(0.,1.,0.));
#18047=DIRECTION('center_axis',(-1.,0.,0.));
#18048=DIRECTION('ref_axis',(0.,-1.,0.));
#18049=DIRECTION('center_axis',(-1.,0.,0.));
#18050=DIRECTION('ref_axis',(0.,1.,0.));
#18051=DIRECTION('center_axis',(-1.,0.,0.));
#18052=DIRECTION('ref_axis',(0.,-1.,0.));
#18053=DIRECTION('center_axis',(-1.,0.,0.));
#18054=DIRECTION('ref_axis',(0.,1.,0.));
#18055=DIRECTION('center_axis',(-1.,0.,0.));
#18056=DIRECTION('ref_axis',(0.,-1.,0.));
#18057=DIRECTION('center_axis',(-1.,0.,0.));
#18058=DIRECTION('ref_axis',(0.,1.,0.));
#18059=DIRECTION('center_axis',(-1.,0.,0.));
#18060=DIRECTION('ref_axis',(0.,-1.,0.));
#18061=DIRECTION('center_axis',(-1.,0.,0.));
#18062=DIRECTION('ref_axis',(0.,1.,0.));
#18063=DIRECTION('center_axis',(-1.,0.,0.));
#18064=DIRECTION('ref_axis',(0.,-1.,0.));
#18065=DIRECTION('center_axis',(-1.,0.,0.));
#18066=DIRECTION('ref_axis',(0.,1.,0.));
#18067=DIRECTION('center_axis',(-1.,0.,0.));
#18068=DIRECTION('ref_axis',(0.,-1.,0.));
#18069=DIRECTION('center_axis',(-1.,0.,0.));
#18070=DIRECTION('ref_axis',(0.,1.,0.));
#18071=DIRECTION('center_axis',(-1.,0.,0.));
#18072=DIRECTION('ref_axis',(0.,-1.,0.));
#18073=DIRECTION('center_axis',(-1.,0.,0.));
#18074=DIRECTION('ref_axis',(0.,1.,0.));
#18075=DIRECTION('center_axis',(-1.,0.,0.));
#18076=DIRECTION('ref_axis',(0.,-1.,0.));
#18077=DIRECTION('center_axis',(-1.,0.,0.));
#18078=DIRECTION('ref_axis',(0.,1.,0.));
#18079=DIRECTION('center_axis',(-1.,0.,0.));
#18080=DIRECTION('ref_axis',(0.,-1.,0.));
#18081=DIRECTION('center_axis',(-1.,0.,0.));
#18082=DIRECTION('ref_axis',(0.,1.,0.));
#18083=DIRECTION('center_axis',(-1.,0.,0.));
#18084=DIRECTION('ref_axis',(0.,-1.,0.));
#18085=DIRECTION('center_axis',(-1.,0.,0.));
#18086=DIRECTION('ref_axis',(0.,1.,0.));
#18087=DIRECTION('center_axis',(-1.,0.,0.));
#18088=DIRECTION('ref_axis',(0.,-1.,0.));
#18089=DIRECTION('center_axis',(-1.,0.,0.));
#18090=DIRECTION('ref_axis',(0.,1.,0.));
#18091=DIRECTION('center_axis',(-1.,0.,0.));
#18092=DIRECTION('ref_axis',(0.,-1.,0.));
#18093=DIRECTION('center_axis',(-1.,0.,0.));
#18094=DIRECTION('ref_axis',(0.,1.,0.));
#18095=DIRECTION('center_axis',(-1.,0.,0.));
#18096=DIRECTION('ref_axis',(0.,-1.,0.));
#18097=DIRECTION('center_axis',(-1.,0.,0.));
#18098=DIRECTION('ref_axis',(0.,1.,0.));
#18099=DIRECTION('center_axis',(-1.,0.,0.));
#18100=DIRECTION('ref_axis',(0.,-1.,0.));
#18101=DIRECTION('center_axis',(-1.,0.,0.));
#18102=DIRECTION('ref_axis',(0.,1.,0.));
#18103=DIRECTION('center_axis',(-1.,0.,0.));
#18104=DIRECTION('ref_axis',(0.,-1.,0.));
#18105=DIRECTION('center_axis',(-1.,0.,0.));
#18106=DIRECTION('ref_axis',(0.,1.,0.));
#18107=DIRECTION('center_axis',(-1.,0.,0.));
#18108=DIRECTION('ref_axis',(0.,-1.,0.));
#18109=DIRECTION('center_axis',(-1.,0.,0.));
#18110=DIRECTION('ref_axis',(0.,1.,0.));
#18111=DIRECTION('center_axis',(-1.,0.,0.));
#18112=DIRECTION('ref_axis',(0.,-1.,0.));
#18113=DIRECTION('center_axis',(-1.,0.,0.));
#18114=DIRECTION('ref_axis',(0.,1.,0.));
#18115=DIRECTION('center_axis',(-1.,0.,0.));
#18116=DIRECTION('ref_axis',(0.,-1.,0.));
#18117=DIRECTION('center_axis',(-1.,0.,0.));
#18118=DIRECTION('ref_axis',(0.,1.,0.));
#18119=DIRECTION('center_axis',(-1.,0.,0.));
#18120=DIRECTION('ref_axis',(0.,-1.,0.));
#18121=DIRECTION('center_axis',(1.,0.,0.));
#18122=DIRECTION('ref_axis',(0.,1.,0.));
#18123=DIRECTION('center_axis',(1.,0.,0.));
#18124=DIRECTION('ref_axis',(0.,0.,-1.));
#18125=DIRECTION('',(-1.,0.,0.));
#18126=DIRECTION('center_axis',(1.,0.,0.));
#18127=DIRECTION('ref_axis',(0.,1.,0.));
#18128=DIRECTION('',(-1.,0.,0.));
#18129=DIRECTION('',(1.,0.,0.));
#18130=DIRECTION('center_axis',(1.,0.,0.));
#18131=DIRECTION('ref_axis',(0.,1.,0.));
#18132=DIRECTION('',(-1.,0.,0.));
#18133=DIRECTION('',(1.,0.,0.));
#18134=DIRECTION('center_axis',(1.,0.,0.));
#18135=DIRECTION('ref_axis',(0.,1.,0.));
#18136=DIRECTION('',(-1.,0.,0.));
#18137=DIRECTION('',(1.,0.,0.));
#18138=DIRECTION('center_axis',(1.,0.,0.));
#18139=DIRECTION('ref_axis',(0.,1.,0.));
#18140=DIRECTION('',(-1.,0.,0.));
#18141=DIRECTION('',(1.,0.,0.));
#18142=DIRECTION('center_axis',(1.,0.,0.));
#18143=DIRECTION('ref_axis',(0.,1.,0.));
#18144=DIRECTION('',(-1.,0.,0.));
#18145=DIRECTION('',(1.,0.,0.));
#18146=DIRECTION('center_axis',(1.,0.,0.));
#18147=DIRECTION('ref_axis',(0.,1.,0.));
#18148=DIRECTION('',(-1.,0.,0.));
#18149=DIRECTION('',(1.,0.,0.));
#18150=DIRECTION('center_axis',(1.,0.,0.));
#18151=DIRECTION('ref_axis',(0.,1.,0.));
#18152=DIRECTION('',(-1.,0.,0.));
#18153=DIRECTION('',(1.,0.,0.));
#18154=DIRECTION('center_axis',(1.,0.,0.));
#18155=DIRECTION('ref_axis',(0.,1.,0.));
#18156=DIRECTION('',(-1.,0.,0.));
#18157=DIRECTION('',(1.,0.,0.));
#18158=DIRECTION('center_axis',(1.,0.,0.));
#18159=DIRECTION('ref_axis',(0.,1.,0.));
#18160=DIRECTION('',(-1.,0.,0.));
#18161=DIRECTION('',(1.,0.,0.));
#18162=DIRECTION('center_axis',(1.,0.,0.));
#18163=DIRECTION('ref_axis',(0.,1.,0.));
#18164=DIRECTION('',(-1.,0.,0.));
#18165=DIRECTION('',(1.,0.,0.));
#18166=DIRECTION('center_axis',(1.,0.,0.));
#18167=DIRECTION('ref_axis',(0.,1.,0.));
#18168=DIRECTION('',(-1.,0.,0.));
#18169=DIRECTION('',(1.,0.,0.));
#18170=DIRECTION('center_axis',(1.,0.,0.));
#18171=DIRECTION('ref_axis',(0.,1.,0.));
#18172=DIRECTION('',(-1.,0.,0.));
#18173=DIRECTION('',(1.,0.,0.));
#18174=DIRECTION('center_axis',(1.,0.,0.));
#18175=DIRECTION('ref_axis',(0.,1.,0.));
#18176=DIRECTION('',(-1.,0.,0.));
#18177=DIRECTION('',(1.,0.,0.));
#18178=DIRECTION('center_axis',(1.,0.,0.));
#18179=DIRECTION('ref_axis',(0.,1.,0.));
#18180=DIRECTION('',(-1.,0.,0.));
#18181=DIRECTION('',(1.,0.,0.));
#18182=DIRECTION('center_axis',(1.,0.,0.));
#18183=DIRECTION('ref_axis',(0.,1.,0.));
#18184=DIRECTION('',(-1.,0.,0.));
#18185=DIRECTION('',(1.,0.,0.));
#18186=DIRECTION('center_axis',(1.,0.,0.));
#18187=DIRECTION('ref_axis',(0.,1.,0.));
#18188=DIRECTION('',(-1.,0.,0.));
#18189=DIRECTION('',(1.,0.,0.));
#18190=DIRECTION('center_axis',(1.,0.,0.));
#18191=DIRECTION('ref_axis',(0.,1.,0.));
#18192=DIRECTION('',(-1.,0.,0.));
#18193=DIRECTION('',(1.,0.,0.));
#18194=DIRECTION('center_axis',(1.,0.,0.));
#18195=DIRECTION('ref_axis',(0.,1.,0.));
#18196=DIRECTION('',(-1.,0.,0.));
#18197=DIRECTION('',(1.,0.,0.));
#18198=DIRECTION('center_axis',(1.,0.,0.));
#18199=DIRECTION('ref_axis',(0.,1.,0.));
#18200=DIRECTION('',(-1.,0.,0.));
#18201=DIRECTION('',(1.,0.,0.));
#18202=DIRECTION('center_axis',(1.,0.,0.));
#18203=DIRECTION('ref_axis',(0.,1.,0.));
#18204=DIRECTION('',(-1.,0.,0.));
#18205=DIRECTION('',(1.,0.,0.));
#18206=DIRECTION('center_axis',(1.,0.,0.));
#18207=DIRECTION('ref_axis',(0.,1.,0.));
#18208=DIRECTION('',(-1.,0.,0.));
#18209=DIRECTION('',(1.,0.,0.));
#18210=DIRECTION('center_axis',(1.,0.,0.));
#18211=DIRECTION('ref_axis',(0.,1.,0.));
#18212=DIRECTION('',(-1.,0.,0.));
#18213=DIRECTION('',(1.,0.,0.));
#18214=DIRECTION('center_axis',(1.,0.,0.));
#18215=DIRECTION('ref_axis',(0.,1.,0.));
#18216=DIRECTION('',(-1.,0.,0.));
#18217=DIRECTION('',(1.,0.,0.));
#18218=DIRECTION('center_axis',(1.,0.,0.));
#18219=DIRECTION('ref_axis',(0.,1.,0.));
#18220=DIRECTION('',(-1.,0.,0.));
#18221=DIRECTION('',(1.,0.,0.));
#18222=DIRECTION('center_axis',(1.,0.,0.));
#18223=DIRECTION('ref_axis',(0.,1.,0.));
#18224=DIRECTION('center_axis',(-1.,0.,0.));
#18225=DIRECTION('ref_axis',(0.,0.,1.));
#18226=DIRECTION('center_axis',(1.,0.,0.));
#18227=DIRECTION('ref_axis',(0.,1.,0.));
#18228=DIRECTION('center_axis',(1.,0.,0.));
#18229=DIRECTION('ref_axis',(0.,0.,-1.));
#18230=DIRECTION('center_axis',(1.,0.,0.));
#18231=DIRECTION('ref_axis',(0.,1.,0.));
#18232=DIRECTION('center_axis',(1.,0.,0.));
#18233=DIRECTION('ref_axis',(0.,1.,0.));
#18234=DIRECTION('center_axis',(-1.,0.,0.));
#18235=DIRECTION('ref_axis',(0.,1.,-9.1414668091865E-14));
#18236=DIRECTION('center_axis',(1.,0.,0.));
#18237=DIRECTION('ref_axis',(0.,1.,-9.1414668091865E-14));
#18238=DIRECTION('center_axis',(0.,-0.372500259691423,0.928032088092768));
#18239=DIRECTION('ref_axis',(0.,-0.928032088092767,-0.372500259691423));
#18240=DIRECTION('',(0.,-0.928032088092767,-0.372500259691423));
#18241=DIRECTION('',(1.,0.,0.));
#18242=DIRECTION('',(0.,-0.928032088092767,-0.372500259691423));
#18243=DIRECTION('center_axis',(1.,0.,0.));
#18244=DIRECTION('ref_axis',(0.,-0.258819045102522,-0.965925826289068));
#18245=DIRECTION('',(0.,0.617449233969742,-0.786610731855458));
#18246=DIRECTION('center_axis',(0.,-0.786610731855458,-0.617449233969742));
#18247=DIRECTION('ref_axis',(0.,0.617449233969742,-0.786610731855458));
#18248=DIRECTION('',(0.,0.617449233969742,-0.786610731855458));
#18249=DIRECTION('center_axis',(1.,0.,0.));
#18250=DIRECTION('ref_axis',(0.,-0.258819045102522,-0.965925826289068));
#18251=DIRECTION('center_axis',(0.,-0.119615242270662,0.992820323027551));
#18252=DIRECTION('ref_axis',(0.,-0.992820323027551,-0.119615242270662));
#18253=DIRECTION('',(0.,-0.992820323027551,-0.119615242270662));
#18254=DIRECTION('',(1.,0.,0.));
#18255=DIRECTION('',(0.,-0.992820323027551,-0.119615242270662));
#18256=DIRECTION('center_axis',(1.,0.,0.));
#18257=DIRECTION('ref_axis',(0.,-0.5,-0.866025403784438));
#18258=DIRECTION('',(0.,0.392820323027551,-0.919615242270663));
#18259=DIRECTION('center_axis',(0.,-0.919615242270663,-0.392820323027551));
#18260=DIRECTION('ref_axis',(0.,0.392820323027551,-0.919615242270663));
#18261=DIRECTION('',(0.,0.392820323027551,-0.919615242270663));
#18262=DIRECTION('center_axis',(1.,0.,0.));
#18263=DIRECTION('ref_axis',(0.,-0.5,-0.866025403784438));
#18264=DIRECTION('center_axis',(0.,0.14142135623731,0.989949493661166));
#18265=DIRECTION('ref_axis',(0.,-0.989949493661166,0.14142135623731));
#18266=DIRECTION('',(0.,-0.989949493661166,0.14142135623731));
#18267=DIRECTION('',(1.,0.,0.));
#18268=DIRECTION('',(0.,-0.989949493661166,0.14142135623731));
#18269=DIRECTION('center_axis',(1.,0.,0.));
#18270=DIRECTION('ref_axis',(0.,-0.707106781186548,-0.707106781186547));
#18271=DIRECTION('',(0.,0.14142135623731,-0.989949493661167));
#18272=DIRECTION('center_axis',(0.,-0.989949493661167,-0.14142135623731));
#18273=DIRECTION('ref_axis',(0.,0.14142135623731,-0.989949493661167));
#18274=DIRECTION('',(0.,0.14142135623731,-0.989949493661167));
#18275=DIRECTION('center_axis',(1.,0.,0.));
#18276=DIRECTION('ref_axis',(0.,-0.707106781186548,-0.707106781186547));
#18277=DIRECTION('center_axis',(0.,0.392820323027552,0.919615242270663));
#18278=DIRECTION('ref_axis',(0.,-0.919615242270663,0.392820323027552));
#18279=DIRECTION('',(0.,-0.919615242270663,0.392820323027552));
#18280=DIRECTION('',(1.,0.,0.));
#18281=DIRECTION('',(0.,-0.919615242270663,0.392820323027552));
#18282=DIRECTION('center_axis',(1.,0.,0.));
#18283=DIRECTION('ref_axis',(0.,-0.866025403784439,-0.499999999999999));
#18284=DIRECTION('',(0.,-0.119615242270664,-0.992820323027551));
#18285=DIRECTION('center_axis',(0.,-0.992820323027551,0.119615242270664));
#18286=DIRECTION('ref_axis',(0.,-0.119615242270664,-0.992820323027551));
#18287=DIRECTION('',(0.,-0.119615242270664,-0.992820323027551));
#18288=DIRECTION('center_axis',(1.,0.,0.));
#18289=DIRECTION('ref_axis',(0.,-0.866025403784439,-0.499999999999999));
#18290=DIRECTION('center_axis',(0.,0.617449233969743,0.786610731855457));
#18291=DIRECTION('ref_axis',(0.,-0.786610731855457,0.617449233969743));
#18292=DIRECTION('',(0.,-0.786610731855457,0.617449233969743));
#18293=DIRECTION('',(1.,0.,0.));
#18294=DIRECTION('',(0.,-0.786610731855457,0.617449233969743));
#18295=DIRECTION('center_axis',(1.,0.,0.));
#18296=DIRECTION('ref_axis',(0.,-0.965925826289068,-0.25881904510252));
#18297=DIRECTION('',(0.,-0.372500259691424,-0.928032088092767));
#18298=DIRECTION('center_axis',(0.,-0.928032088092767,0.372500259691424));
#18299=DIRECTION('ref_axis',(0.,-0.372500259691424,-0.928032088092767));
#18300=DIRECTION('',(0.,-0.372500259691424,-0.928032088092767));
#18301=DIRECTION('center_axis',(1.,0.,0.));
#18302=DIRECTION('ref_axis',(0.,-0.965925826289068,-0.25881904510252));
#18303=DIRECTION('center_axis',(0.,0.8,0.6));
#18304=DIRECTION('ref_axis',(0.,-0.6,0.8));
#18305=DIRECTION('',(0.,-0.6,0.8));
#18306=DIRECTION('',(1.,0.,0.));
#18307=DIRECTION('',(0.,-0.6,0.8));
#18308=DIRECTION('center_axis',(1.,0.,0.));
#18309=DIRECTION('ref_axis',(0.,-1.,1.83697019872103E-16));
#18310=DIRECTION('',(0.,-0.6,-0.8));
#18311=DIRECTION('center_axis',(0.,-0.8,0.6));
#18312=DIRECTION('ref_axis',(0.,-0.6,-0.8));
#18313=DIRECTION('',(0.,-0.6,-0.8));
#18314=DIRECTION('center_axis',(1.,0.,0.));
#18315=DIRECTION('ref_axis',(0.,-1.,1.83697019872103E-16));
#18316=DIRECTION('center_axis',(0.,0.928032088092767,0.372500259691423));
#18317=DIRECTION('ref_axis',(0.,-0.372500259691423,0.928032088092767));
#18318=DIRECTION('',(0.,-0.372500259691423,0.928032088092767));
#18319=DIRECTION('',(1.,0.,0.));
#18320=DIRECTION('',(0.,-0.372500259691423,0.928032088092767));
#18321=DIRECTION('center_axis',(1.,0.,0.));
#18322=DIRECTION('ref_axis',(0.,-0.965925826289068,0.258819045102522));
#18323=DIRECTION('',(0.,-0.786610731855458,-0.617449233969742));
#18324=DIRECTION('center_axis',(0.,-0.617449233969742,0.786610731855458));
#18325=DIRECTION('ref_axis',(0.,-0.786610731855458,-0.617449233969742));
#18326=DIRECTION('',(0.,-0.786610731855458,-0.617449233969742));
#18327=DIRECTION('center_axis',(1.,0.,0.));
#18328=DIRECTION('ref_axis',(0.,-0.965925826289068,0.258819045102522));
#18329=DIRECTION('center_axis',(0.,0.992820323027551,0.119615242270662));
#18330=DIRECTION('ref_axis',(0.,-0.119615242270662,0.992820323027551));
#18331=DIRECTION('',(0.,-0.119615242270662,0.992820323027551));
#18332=DIRECTION('',(1.,0.,0.));
#18333=DIRECTION('',(0.,-0.119615242270662,0.992820323027551));
#18334=DIRECTION('center_axis',(1.,0.,0.));
#18335=DIRECTION('ref_axis',(0.,-0.866025403784438,0.5));
#18336=DIRECTION('',(0.,-0.919615242270663,-0.392820323027551));
#18337=DIRECTION('center_axis',(0.,-0.392820323027551,0.919615242270663));
#18338=DIRECTION('ref_axis',(0.,-0.919615242270663,-0.392820323027551));
#18339=DIRECTION('',(0.,-0.919615242270663,-0.392820323027551));
#18340=DIRECTION('center_axis',(1.,0.,0.));
#18341=DIRECTION('ref_axis',(0.,-0.866025403784438,0.5));
#18342=DIRECTION('center_axis',(0.,0.989949493661166,-0.14142135623731));
#18343=DIRECTION('ref_axis',(0.,0.14142135623731,0.989949493661166));
#18344=DIRECTION('',(0.,0.14142135623731,0.989949493661166));
#18345=DIRECTION('',(1.,0.,0.));
#18346=DIRECTION('',(0.,0.14142135623731,0.989949493661166));
#18347=DIRECTION('center_axis',(1.,0.,0.));
#18348=DIRECTION('ref_axis',(0.,-0.707106781186547,0.707106781186548));
#18349=DIRECTION('',(0.,-0.989949493661167,-0.141421356237309));
#18350=DIRECTION('center_axis',(0.,-0.141421356237309,0.989949493661167));
#18351=DIRECTION('ref_axis',(0.,-0.989949493661167,-0.141421356237309));
#18352=DIRECTION('',(0.,-0.989949493661167,-0.141421356237309));
#18353=DIRECTION('center_axis',(1.,0.,0.));
#18354=DIRECTION('ref_axis',(0.,-0.707106781186547,0.707106781186548));
#18355=DIRECTION('center_axis',(0.,0.919615242270663,-0.392820323027552));
#18356=DIRECTION('ref_axis',(0.,0.392820323027552,0.919615242270663));
#18357=DIRECTION('',(0.,0.392820323027552,0.919615242270663));
#18358=DIRECTION('',(1.,0.,0.));
#18359=DIRECTION('',(0.,0.392820323027552,0.919615242270663));
#18360=DIRECTION('center_axis',(1.,0.,0.));
#18361=DIRECTION('ref_axis',(0.,-0.5,0.866025403784439));
#18362=DIRECTION('',(0.,-0.992820323027551,0.119615242270663));
#18363=DIRECTION('center_axis',(0.,0.119615242270663,0.992820323027551));
#18364=DIRECTION('ref_axis',(0.,-0.992820323027551,0.119615242270663));
#18365=DIRECTION('',(0.,-0.992820323027551,0.119615242270663));
#18366=DIRECTION('center_axis',(1.,0.,0.));
#18367=DIRECTION('ref_axis',(0.,-0.5,0.866025403784439));
#18368=DIRECTION('center_axis',(0.,0.786610731855457,-0.617449233969743));
#18369=DIRECTION('ref_axis',(0.,0.617449233969743,0.786610731855457));
#18370=DIRECTION('',(0.,0.617449233969743,0.786610731855457));
#18371=DIRECTION('',(1.,0.,0.));
#18372=DIRECTION('',(0.,0.617449233969743,0.786610731855457));
#18373=DIRECTION('center_axis',(1.,0.,0.));
#18374=DIRECTION('ref_axis',(0.,-0.25881904510252,0.965925826289068));
#18375=DIRECTION('',(0.,-0.928032088092767,0.372500259691424));
#18376=DIRECTION('center_axis',(0.,0.372500259691424,0.928032088092767));
#18377=DIRECTION('ref_axis',(0.,-0.928032088092767,0.372500259691424));
#18378=DIRECTION('',(0.,-0.928032088092767,0.372500259691424));
#18379=DIRECTION('center_axis',(1.,0.,0.));
#18380=DIRECTION('ref_axis',(0.,-0.25881904510252,0.965925826289068));
#18381=DIRECTION('center_axis',(0.,0.6,-0.8));
#18382=DIRECTION('ref_axis',(0.,0.8,0.6));
#18383=DIRECTION('',(0.,0.8,0.6));
#18384=DIRECTION('',(1.,0.,0.));
#18385=DIRECTION('',(0.,0.8,0.6));
#18386=DIRECTION('center_axis',(1.,0.,0.));
#18387=DIRECTION('ref_axis',(0.,1.22464679914735E-16,1.));
#18388=DIRECTION('',(0.,-0.8,0.6));
#18389=DIRECTION('center_axis',(0.,0.6,0.8));
#18390=DIRECTION('ref_axis',(0.,-0.8,0.6));
#18391=DIRECTION('',(0.,-0.8,0.6));
#18392=DIRECTION('center_axis',(1.,0.,0.));
#18393=DIRECTION('ref_axis',(0.,1.22464679914735E-16,1.));
#18394=DIRECTION('center_axis',(0.,0.372500259691424,-0.928032088092767));
#18395=DIRECTION('ref_axis',(0.,0.928032088092767,0.372500259691424));
#18396=DIRECTION('',(0.,0.928032088092767,0.372500259691424));
#18397=DIRECTION('',(1.,0.,0.));
#18398=DIRECTION('',(0.,0.928032088092767,0.372500259691424));
#18399=DIRECTION('center_axis',(1.,0.,0.));
#18400=DIRECTION('ref_axis',(0.,0.258819045102521,0.965925826289068));
#18401=DIRECTION('',(0.,-0.617449233969742,0.786610731855457));
#18402=DIRECTION('center_axis',(0.,0.786610731855457,0.617449233969742));
#18403=DIRECTION('ref_axis',(0.,-0.617449233969742,0.786610731855457));
#18404=DIRECTION('',(0.,-0.617449233969742,0.786610731855457));
#18405=DIRECTION('center_axis',(1.,0.,0.));
#18406=DIRECTION('ref_axis',(0.,0.258819045102521,0.965925826289068));
#18407=DIRECTION('center_axis',(0.,0.119615242270662,-0.992820323027551));
#18408=DIRECTION('ref_axis',(0.,0.992820323027551,0.119615242270662));
#18409=DIRECTION('',(0.,0.992820323027551,0.119615242270662));
#18410=DIRECTION('',(1.,0.,0.));
#18411=DIRECTION('',(0.,0.992820323027551,0.119615242270662));
#18412=DIRECTION('center_axis',(1.,0.,0.));
#18413=DIRECTION('ref_axis',(0.,0.5,0.866025403784438));
#18414=DIRECTION('',(0.,-0.392820323027551,0.919615242270663));
#18415=DIRECTION('center_axis',(0.,0.919615242270663,0.392820323027551));
#18416=DIRECTION('ref_axis',(0.,-0.392820323027551,0.919615242270663));
#18417=DIRECTION('',(0.,-0.392820323027551,0.919615242270663));
#18418=DIRECTION('center_axis',(1.,0.,0.));
#18419=DIRECTION('ref_axis',(0.,0.5,0.866025403784438));
#18420=DIRECTION('center_axis',(0.,-0.14142135623731,-0.989949493661166));
#18421=DIRECTION('ref_axis',(0.,0.989949493661166,-0.14142135623731));
#18422=DIRECTION('',(0.,0.989949493661166,-0.14142135623731));
#18423=DIRECTION('',(1.,0.,0.));
#18424=DIRECTION('',(0.,0.989949493661166,-0.14142135623731));
#18425=DIRECTION('center_axis',(1.,0.,0.));
#18426=DIRECTION('ref_axis',(0.,0.707106781186548,0.707106781186547));
#18427=DIRECTION('',(0.,-0.14142135623731,0.989949493661167));
#18428=DIRECTION('center_axis',(0.,0.989949493661166,0.14142135623731));
#18429=DIRECTION('ref_axis',(0.,-0.14142135623731,0.989949493661167));
#18430=DIRECTION('',(0.,-0.14142135623731,0.989949493661167));
#18431=DIRECTION('center_axis',(1.,0.,0.));
#18432=DIRECTION('ref_axis',(0.,0.707106781186548,0.707106781186547));
#18433=DIRECTION('center_axis',(0.,-0.392820323027552,-0.919615242270663));
#18434=DIRECTION('ref_axis',(0.,0.919615242270663,-0.392820323027551));
#18435=DIRECTION('',(0.,0.919615242270663,-0.392820323027551));
#18436=DIRECTION('',(1.,0.,0.));
#18437=DIRECTION('',(0.,0.919615242270663,-0.392820323027551));
#18438=DIRECTION('center_axis',(1.,0.,0.));
#18439=DIRECTION('ref_axis',(0.,0.866025403784439,0.5));
#18440=DIRECTION('',(0.,0.119615242270663,0.992820323027551));
#18441=DIRECTION('center_axis',(0.,0.992820323027551,-0.119615242270663));
#18442=DIRECTION('ref_axis',(0.,0.119615242270663,0.992820323027551));
#18443=DIRECTION('',(0.,0.119615242270663,0.992820323027551));
#18444=DIRECTION('center_axis',(1.,0.,0.));
#18445=DIRECTION('ref_axis',(0.,0.866025403784439,0.5));
#18446=DIRECTION('center_axis',(0.,-0.617449233969743,-0.786610731855457));
#18447=DIRECTION('ref_axis',(0.,0.786610731855457,-0.617449233969743));
#18448=DIRECTION('',(0.,0.786610731855457,-0.617449233969743));
#18449=DIRECTION('',(1.,0.,0.));
#18450=DIRECTION('',(0.,0.786610731855457,-0.617449233969743));
#18451=DIRECTION('center_axis',(1.,0.,0.));
#18452=DIRECTION('ref_axis',(0.,0.965925826289068,0.258819045102521));
#18453=DIRECTION('',(0.,0.372500259691424,0.928032088092767));
#18454=DIRECTION('center_axis',(0.,0.928032088092767,-0.372500259691424));
#18455=DIRECTION('ref_axis',(0.,0.372500259691424,0.928032088092767));
#18456=DIRECTION('',(0.,0.372500259691424,0.928032088092767));
#18457=DIRECTION('center_axis',(1.,0.,0.));
#18458=DIRECTION('ref_axis',(0.,0.965925826289068,0.258819045102521));
#18459=DIRECTION('center_axis',(0.,-0.8,-0.6));
#18460=DIRECTION('ref_axis',(0.,0.6,-0.8));
#18461=DIRECTION('',(0.,0.6,-0.8));
#18462=DIRECTION('',(1.,0.,0.));
#18463=DIRECTION('',(0.,0.6,-0.8));
#18464=DIRECTION('center_axis',(1.,0.,0.));
#18465=DIRECTION('ref_axis',(0.,1.,-6.12323399573677E-17));
#18466=DIRECTION('',(0.,0.6,0.8));
#18467=DIRECTION('center_axis',(0.,0.8,-0.6));
#18468=DIRECTION('ref_axis',(0.,0.6,0.8));
#18469=DIRECTION('',(0.,0.6,0.8));
#18470=DIRECTION('center_axis',(1.,0.,0.));
#18471=DIRECTION('ref_axis',(0.,1.,-6.12323399573677E-17));
#18472=DIRECTION('center_axis',(0.,-0.928032088092767,-0.372500259691424));
#18473=DIRECTION('ref_axis',(0.,0.372500259691424,-0.928032088092767));
#18474=DIRECTION('',(0.,0.372500259691424,-0.928032088092767));
#18475=DIRECTION('',(1.,0.,0.));
#18476=DIRECTION('',(0.,0.372500259691424,-0.928032088092767));
#18477=DIRECTION('center_axis',(1.,0.,0.));
#18478=DIRECTION('ref_axis',(0.,0.965925826289068,-0.258819045102521));
#18479=DIRECTION('',(0.,0.786610731855457,0.617449233969742));
#18480=DIRECTION('center_axis',(0.,0.617449233969742,-0.786610731855457));
#18481=DIRECTION('ref_axis',(0.,0.786610731855457,0.617449233969742));
#18482=DIRECTION('',(0.,0.786610731855457,0.617449233969742));
#18483=DIRECTION('center_axis',(1.,0.,0.));
#18484=DIRECTION('ref_axis',(0.,0.965925826289068,-0.258819045102521));
#18485=DIRECTION('center_axis',(0.,-0.992820323027551,-0.119615242270663));
#18486=DIRECTION('ref_axis',(0.,0.119615242270663,-0.992820323027551));
#18487=DIRECTION('',(0.,0.119615242270663,-0.992820323027551));
#18488=DIRECTION('',(1.,0.,0.));
#18489=DIRECTION('',(0.,0.119615242270663,-0.992820323027551));
#18490=DIRECTION('center_axis',(1.,0.,0.));
#18491=DIRECTION('ref_axis',(0.,0.866025403784439,-0.5));
#18492=DIRECTION('',(0.,0.919615242270663,0.392820323027551));
#18493=DIRECTION('center_axis',(0.,0.392820323027551,-0.919615242270663));
#18494=DIRECTION('ref_axis',(0.,0.919615242270663,0.392820323027551));
#18495=DIRECTION('',(0.,0.919615242270663,0.392820323027551));
#18496=DIRECTION('center_axis',(1.,0.,0.));
#18497=DIRECTION('ref_axis',(0.,0.866025403784439,-0.5));
#18498=DIRECTION('center_axis',(0.,-0.989949493661167,0.14142135623731));
#18499=DIRECTION('ref_axis',(0.,-0.14142135623731,-0.989949493661167));
#18500=DIRECTION('',(0.,-0.14142135623731,-0.989949493661167));
#18501=DIRECTION('',(1.,0.,0.));
#18502=DIRECTION('',(0.,-0.14142135623731,-0.989949493661167));
#18503=DIRECTION('center_axis',(1.,0.,0.));
#18504=DIRECTION('ref_axis',(0.,0.707106781186548,-0.707106781186548));
#18505=DIRECTION('',(0.,0.989949493661167,0.14142135623731));
#18506=DIRECTION('center_axis',(0.,0.14142135623731,-0.989949493661167));
#18507=DIRECTION('ref_axis',(0.,0.989949493661167,0.14142135623731));
#18508=DIRECTION('',(0.,0.989949493661167,0.14142135623731));
#18509=DIRECTION('center_axis',(1.,0.,0.));
#18510=DIRECTION('ref_axis',(0.,0.707106781186548,-0.707106781186548));
#18511=DIRECTION('center_axis',(0.,-0.919615242270663,0.392820323027551));
#18512=DIRECTION('ref_axis',(0.,-0.392820323027551,-0.919615242270663));
#18513=DIRECTION('',(0.,-0.392820323027551,-0.919615242270663));
#18514=DIRECTION('',(1.,0.,0.));
#18515=DIRECTION('',(0.,-0.392820323027551,-0.919615242270663));
#18516=DIRECTION('center_axis',(1.,0.,0.));
#18517=DIRECTION('ref_axis',(0.,0.5,-0.866025403784439));
#18518=DIRECTION('',(0.,0.992820323027551,-0.119615242270663));
#18519=DIRECTION('center_axis',(0.,-0.119615242270663,-0.992820323027551));
#18520=DIRECTION('ref_axis',(0.,0.992820323027551,-0.119615242270663));
#18521=DIRECTION('',(0.,0.992820323027551,-0.119615242270663));
#18522=DIRECTION('center_axis',(1.,0.,0.));
#18523=DIRECTION('ref_axis',(0.,0.5,-0.866025403784439));
#18524=DIRECTION('center_axis',(0.,-0.786610731855457,0.617449233969743));
#18525=DIRECTION('ref_axis',(0.,-0.617449233969742,-0.786610731855457));
#18526=DIRECTION('',(0.,-0.617449233969742,-0.786610731855457));
#18527=DIRECTION('',(1.,0.,0.));
#18528=DIRECTION('',(0.,-0.617449233969742,-0.786610731855457));
#18529=DIRECTION('center_axis',(1.,0.,0.));
#18530=DIRECTION('ref_axis',(0.,0.258819045102521,-0.965925826289068));
#18531=DIRECTION('',(0.,0.928032088092767,-0.372500259691424));
#18532=DIRECTION('center_axis',(0.,-0.372500259691424,-0.928032088092767));
#18533=DIRECTION('ref_axis',(0.,0.928032088092767,-0.372500259691424));
#18534=DIRECTION('',(0.,0.928032088092767,-0.372500259691424));
#18535=DIRECTION('center_axis',(1.,0.,0.));
#18536=DIRECTION('ref_axis',(0.,0.258819045102521,-0.965925826289068));
#18537=DIRECTION('center_axis',(0.,-0.6,0.8));
#18538=DIRECTION('ref_axis',(0.,-0.8,-0.6));
#18539=DIRECTION('',(0.,-0.8,-0.6));
#18540=DIRECTION('',(1.,0.,0.));
#18541=DIRECTION('',(0.,-0.8,-0.6));
#18542=DIRECTION('center_axis',(1.,0.,0.));
#18543=DIRECTION('ref_axis',(0.,0.,-1.));
#18544=DIRECTION('',(0.,0.8,-0.6));
#18545=DIRECTION('center_axis',(0.,-0.6,-0.8));
#18546=DIRECTION('ref_axis',(0.,0.8,-0.6));
#18547=DIRECTION('',(0.,0.8,-0.6));
#18548=DIRECTION('center_axis',(1.,0.,0.));
#18549=DIRECTION('ref_axis',(0.,0.,-1.));
#18550=DIRECTION('center_axis',(-1.,0.,0.));
#18551=DIRECTION('ref_axis',(0.,0.,1.));
#18552=DIRECTION('center_axis',(1.,0.,0.));
#18553=DIRECTION('ref_axis',(0.,0.,-1.));
#18554=DIRECTION('center_axis',(1.,0.,0.));
#18555=DIRECTION('ref_axis',(0.,1.,0.));
#18556=DIRECTION('',(-0.707106781186548,0.707106781186548,8.65956056235494E-17));
#18557=DIRECTION('center_axis',(1.,0.,0.));
#18558=DIRECTION('ref_axis',(0.,1.,0.));
#18559=DIRECTION('center_axis',(-1.,0.,0.));
#18560=DIRECTION('ref_axis',(0.,1.,0.));
#18561=DIRECTION('center_axis',(1.,0.,0.));
#18562=DIRECTION('ref_axis',(0.,0.,-1.));
#18563=DIRECTION('',(-0.707106781186549,-0.707106781186546,-8.65956056235491E-17));
#18564=DIRECTION('center_axis',(1.,0.,0.));
#18565=DIRECTION('ref_axis',(0.,0.,-1.));
#18566=DIRECTION('center_axis',(1.,0.,0.));
#18567=DIRECTION('ref_axis',(0.,0.,-1.));
#18568=DIRECTION('center_axis',(1.,0.,0.));
#18569=DIRECTION('ref_axis',(0.,1.,0.));
#18570=DIRECTION('',(-1.,0.,0.));
#18571=DIRECTION('center_axis',(1.,0.,0.));
#18572=DIRECTION('ref_axis',(0.,0.,-1.));
#18573=DIRECTION('center_axis',(1.,0.,0.));
#18574=DIRECTION('ref_axis',(0.,0.,-1.));
#18575=DIRECTION('axis',(0.,0.,1.));
#18576=DIRECTION('refdir',(1.,0.,0.));
#18577=DIRECTION('center_axis',(1.,0.,0.));
#18578=DIRECTION('ref_axis',(0.,-1.,0.));
#18579=DIRECTION('center_axis',(-1.,0.,0.));
#18580=DIRECTION('ref_axis',(0.,-1.,0.));
#18581=DIRECTION('center_axis',(-1.,0.,0.));
#18582=DIRECTION('ref_axis',(0.,-1.,0.));
#18583=DIRECTION('',(0.707106781186548,0.707106781186547,-8.65956056235493E-17));
#18584=DIRECTION('center_axis',(1.,0.,0.));
#18585=DIRECTION('ref_axis',(0.,-1.,0.));
#18586=DIRECTION('center_axis',(1.,0.,0.));
#18587=DIRECTION('ref_axis',(0.,1.,0.));
#18588=DIRECTION('',(-1.,0.,0.));
#18589=DIRECTION('center_axis',(1.,0.,0.));
#18590=DIRECTION('ref_axis',(0.,1.,0.));
#18591=DIRECTION('center_axis',(1.,0.,0.));
#18592=DIRECTION('ref_axis',(0.,0.,-1.));
#18593=DIRECTION('center_axis',(1.,0.,0.));
#18594=DIRECTION('ref_axis',(0.,0.,-1.));
#18595=DIRECTION('center_axis',(0.,0.946649377085496,0.322265351633779));
#18596=DIRECTION('ref_axis',(0.,-0.322265351633779,0.946649377085496));
#18597=DIRECTION('',(-1.,0.,0.));
#18598=DIRECTION('',(0.,0.322265351633779,-0.946649377085496));
#18599=DIRECTION('',(1.,0.,0.));
#18600=DIRECTION('center_axis',(1.,0.,0.));
#18601=DIRECTION('ref_axis',(0.,1.,0.));
#18602=DIRECTION('center_axis',(-1.,0.,0.));
#18603=DIRECTION('ref_axis',(0.,1.,0.));
#18604=DIRECTION('center_axis',(1.,0.,0.));
#18605=DIRECTION('ref_axis',(0.,0.,-1.));
#18606=DIRECTION('',(1.,0.,0.));
#18607=DIRECTION('center_axis',(-1.,0.,0.));
#18608=DIRECTION('ref_axis',(0.,1.,0.));
#18609=DIRECTION('',(-1.,0.,0.));
#18610=DIRECTION('center_axis',(1.,0.,0.));
#18611=DIRECTION('ref_axis',(0.,0.,-1.));
#18612=DIRECTION('',(1.,0.,0.));
#18613=DIRECTION('center_axis',(-1.,0.,0.));
#18614=DIRECTION('ref_axis',(0.,1.,0.));
#18615=DIRECTION('',(-1.,0.,0.));
#18616=DIRECTION('center_axis',(1.,0.,0.));
#18617=DIRECTION('ref_axis',(0.,0.,-1.));
#18618=DIRECTION('',(1.,0.,0.));
#18619=DIRECTION('center_axis',(-1.,0.,0.));
#18620=DIRECTION('ref_axis',(0.,1.,0.));
#18621=DIRECTION('',(-1.,0.,0.));
#18622=DIRECTION('center_axis',(1.,0.,0.));
#18623=DIRECTION('ref_axis',(0.,0.,-1.));
#18624=DIRECTION('',(1.,0.,0.));
#18625=DIRECTION('center_axis',(-1.,0.,0.));
#18626=DIRECTION('ref_axis',(0.,1.,0.));
#18627=DIRECTION('',(-1.,0.,0.));
#18628=DIRECTION('center_axis',(1.,0.,0.));
#18629=DIRECTION('ref_axis',(0.,0.,-1.));
#18630=DIRECTION('',(1.,0.,0.));
#18631=DIRECTION('center_axis',(-1.,0.,0.));
#18632=DIRECTION('ref_axis',(0.,1.,0.));
#18633=DIRECTION('',(-1.,0.,0.));
#18634=DIRECTION('center_axis',(1.,0.,0.));
#18635=DIRECTION('ref_axis',(0.,0.,-1.));
#18636=DIRECTION('',(1.,0.,0.));
#18637=DIRECTION('center_axis',(-1.,0.,0.));
#18638=DIRECTION('ref_axis',(0.,1.,0.));
#18639=DIRECTION('',(-1.,0.,0.));
#18640=DIRECTION('center_axis',(1.,0.,0.));
#18641=DIRECTION('ref_axis',(0.,0.,-1.));
#18642=DIRECTION('',(1.,0.,0.));
#18643=DIRECTION('center_axis',(-1.,0.,0.));
#18644=DIRECTION('ref_axis',(0.,1.,0.));
#18645=DIRECTION('',(-1.,0.,0.));
#18646=DIRECTION('center_axis',(1.,0.,0.));
#18647=DIRECTION('ref_axis',(0.,0.,-1.));
#18648=DIRECTION('',(1.,0.,0.));
#18649=DIRECTION('center_axis',(-1.,0.,0.));
#18650=DIRECTION('ref_axis',(0.,1.,0.));
#18651=DIRECTION('',(-1.,0.,0.));
#18652=DIRECTION('center_axis',(1.,0.,0.));
#18653=DIRECTION('ref_axis',(0.,0.,-1.));
#18654=DIRECTION('center_axis',(-1.,0.,0.));
#18655=DIRECTION('ref_axis',(0.,1.,0.));
#18656=DIRECTION('',(-1.,0.,0.));
#18657=DIRECTION('center_axis',(1.,0.,0.));
#18658=DIRECTION('ref_axis',(0.,0.,-1.));
#18659=DIRECTION('',(1.,0.,0.));
#18660=DIRECTION('center_axis',(-1.,0.,0.));
#18661=DIRECTION('ref_axis',(0.,1.,0.));
#18662=DIRECTION('',(-1.,0.,0.));
#18663=DIRECTION('center_axis',(1.,0.,0.));
#18664=DIRECTION('ref_axis',(0.,0.,-1.));
#18665=DIRECTION('',(1.,0.,0.));
#18666=DIRECTION('center_axis',(-1.,0.,0.));
#18667=DIRECTION('ref_axis',(0.,1.,0.));
#18668=DIRECTION('',(-1.,0.,0.));
#18669=DIRECTION('center_axis',(1.,0.,0.));
#18670=DIRECTION('ref_axis',(0.,0.,-1.));
#18671=DIRECTION('',(1.,0.,0.));
#18672=DIRECTION('center_axis',(-1.,0.,0.));
#18673=DIRECTION('ref_axis',(0.,1.,0.));
#18674=DIRECTION('',(-1.,0.,0.));
#18675=DIRECTION('center_axis',(1.,0.,0.));
#18676=DIRECTION('ref_axis',(0.,0.,-1.));
#18677=DIRECTION('',(1.,0.,0.));
#18678=DIRECTION('center_axis',(-1.,0.,0.));
#18679=DIRECTION('ref_axis',(0.,1.,0.));
#18680=DIRECTION('',(-1.,0.,0.));
#18681=DIRECTION('center_axis',(1.,0.,0.));
#18682=DIRECTION('ref_axis',(0.,0.,-1.));
#18683=DIRECTION('',(1.,0.,0.));
#18684=DIRECTION('center_axis',(-1.,0.,0.));
#18685=DIRECTION('ref_axis',(0.,1.,0.));
#18686=DIRECTION('',(-1.,0.,0.));
#18687=DIRECTION('center_axis',(1.,0.,0.));
#18688=DIRECTION('ref_axis',(0.,0.,-1.));
#18689=DIRECTION('',(1.,0.,0.));
#18690=DIRECTION('center_axis',(-1.,0.,0.));
#18691=DIRECTION('ref_axis',(0.,1.,0.));
#18692=DIRECTION('',(-1.,0.,0.));
#18693=DIRECTION('center_axis',(1.,0.,0.));
#18694=DIRECTION('ref_axis',(0.,0.,-1.));
#18695=DIRECTION('',(1.,0.,0.));
#18696=DIRECTION('center_axis',(-1.,0.,0.));
#18697=DIRECTION('ref_axis',(0.,1.,0.));
#18698=DIRECTION('',(-1.,0.,0.));
#18699=DIRECTION('center_axis',(1.,0.,0.));
#18700=DIRECTION('ref_axis',(0.,0.,-1.));
#18701=DIRECTION('',(1.,0.,0.));
#18702=DIRECTION('center_axis',(-1.,0.,0.));
#18703=DIRECTION('ref_axis',(0.,1.,0.));
#18704=DIRECTION('',(-0.707106781186548,-0.707106781186547,-8.65956056235493E-17));
#18705=DIRECTION('center_axis',(0.,0.946649377085496,-0.322265351633779));
#18706=DIRECTION('ref_axis',(0.,0.322265351633779,0.946649377085496));
#18707=DIRECTION('',(-1.,0.,0.));
#18708=DIRECTION('',(0.,-0.322265351633779,-0.946649377085496));
#18709=DIRECTION('center_axis',(0.,0.751264373058291,0.660001395281354));
#18710=DIRECTION('ref_axis',(1.,0.,0.));
#18711=DIRECTION('',(0.,0.660001395281354,-0.751264373058291));
#18712=DIRECTION('',(1.,0.,0.));
#18713=DIRECTION('center_axis',(0.,0.997915594849406,0.0645326704573513));
#18714=DIRECTION('ref_axis',(0.,-0.0645326704573513,0.997915594849406));
#18715=DIRECTION('',(-1.,0.,0.));
#18716=DIRECTION('',(0.,0.0645326704573513,-0.997915594849406));
#18717=DIRECTION('center_axis',(0.,0.441506178461464,0.897258209424887));
#18718=DIRECTION('ref_axis',(1.,0.,0.));
#18719=DIRECTION('',(0.,0.897258209424887,-0.441506178461464));
#18720=DIRECTION('',(1.,0.,0.));
#18721=DIRECTION('center_axis',(0.,0.897258209424887,0.441506178461464));
#18722=DIRECTION('ref_axis',(0.,-0.441506178461464,0.897258209424887));
#18723=DIRECTION('',(-1.,0.,0.));
#18724=DIRECTION('',(0.,0.441506178461464,-0.897258209424887));
#18725=DIRECTION('center_axis',(0.,0.0645326704573477,0.997915594849406));
#18726=DIRECTION('ref_axis',(1.,0.,0.));
#18727=DIRECTION('',(0.,0.997915594849406,-0.0645326704573477));
#18728=DIRECTION('',(1.,0.,0.));
#18729=DIRECTION('center_axis',(0.,0.660001395281354,0.751264373058291));
#18730=DIRECTION('ref_axis',(1.,0.,0.));
#18731=DIRECTION('',(-1.,0.,0.));
#18732=DIRECTION('',(0.,0.751264373058291,-0.660001395281354));
#18733=DIRECTION('center_axis',(0.,-0.322265351633779,0.946649377085496));
#18734=DIRECTION('ref_axis',(1.,0.,0.));
#18735=DIRECTION('',(0.,0.946649377085496,0.322265351633779));
#18736=DIRECTION('',(1.,0.,0.));
#18737=DIRECTION('center_axis',(0.,0.322265351633779,0.946649377085496));
#18738=DIRECTION('ref_axis',(1.,0.,0.));
#18739=DIRECTION('',(-1.,0.,0.));
#18740=DIRECTION('',(0.,0.946649377085496,-0.322265351633779));
#18741=DIRECTION('center_axis',(0.,-0.660001395281353,0.751264373058291));
#18742=DIRECTION('ref_axis',(1.,0.,0.));
#18743=DIRECTION('',(0.,0.751264373058291,0.660001395281353));
#18744=DIRECTION('',(1.,0.,0.));
#18745=DIRECTION('center_axis',(0.,-0.0645326704573494,0.997915594849406));
#18746=DIRECTION('ref_axis',(1.,0.,0.));
#18747=DIRECTION('',(-1.,0.,0.));
#18748=DIRECTION('',(0.,0.997915594849406,0.0645326704573494));
#18749=DIRECTION('center_axis',(0.,-0.897258209424888,0.441506178461462));
#18750=DIRECTION('ref_axis',(0.,-0.441506178461462,-0.897258209424888));
#18751=DIRECTION('',(0.,0.441506178461462,0.897258209424888));
#18752=DIRECTION('',(1.,0.,0.));
#18753=DIRECTION('center_axis',(0.,-0.441506178461463,0.897258209424887));
#18754=DIRECTION('ref_axis',(1.,0.,0.));
#18755=DIRECTION('',(-1.,0.,0.));
#18756=DIRECTION('',(0.,0.897258209424887,0.441506178461463));
#18757=DIRECTION('center_axis',(0.,-0.997915594849406,0.0645326704573477));
#18758=DIRECTION('ref_axis',(0.,-0.0645326704573477,-0.997915594849406));
#18759=DIRECTION('',(0.,0.0645326704573477,0.997915594849406));
#18760=DIRECTION('',(1.,0.,0.));
#18761=DIRECTION('center_axis',(0.,-0.751264373058291,0.660001395281354));
#18762=DIRECTION('ref_axis',(1.,0.,0.));
#18763=DIRECTION('',(-1.,0.,0.));
#18764=DIRECTION('',(0.,0.660001395281354,0.751264373058291));
#18765=DIRECTION('center_axis',(0.,-0.946649377085496,-0.322265351633779));
#18766=DIRECTION('ref_axis',(0.,0.322265351633779,-0.946649377085496));
#18767=DIRECTION('',(0.,-0.322265351633779,0.946649377085496));
#18768=DIRECTION('',(1.,0.,0.));
#18769=DIRECTION('center_axis',(0.,-0.946649377085496,0.322265351633779));
#18770=DIRECTION('ref_axis',(0.,-0.322265351633779,-0.946649377085496));
#18771=DIRECTION('',(-1.,0.,0.));
#18772=DIRECTION('',(0.,0.322265351633779,0.946649377085496));
#18773=DIRECTION('center_axis',(0.,-0.75126437305829,-0.660001395281354));
#18774=DIRECTION('ref_axis',(-1.,0.,0.));
#18775=DIRECTION('',(0.,-0.660001395281354,0.75126437305829));
#18776=DIRECTION('',(1.,0.,0.));
#18777=DIRECTION('center_axis',(0.,-0.997915594849406,-0.0645326704573514));
#18778=DIRECTION('ref_axis',(0.,0.0645326704573514,-0.997915594849406));
#18779=DIRECTION('',(-1.,0.,0.));
#18780=DIRECTION('',(0.,-0.0645326704573514,0.997915594849406));
#18781=DIRECTION('center_axis',(0.,-0.441506178461457,-0.89725820942489));
#18782=DIRECTION('ref_axis',(-1.,0.,0.));
#18783=DIRECTION('',(0.,-0.89725820942489,0.441506178461457));
#18784=DIRECTION('',(1.,0.,0.));
#18785=DIRECTION('center_axis',(0.,-0.89725820942489,-0.441506178461457));
#18786=DIRECTION('ref_axis',(0.,0.441506178461457,-0.89725820942489));
#18787=DIRECTION('',(-1.,0.,0.));
#18788=DIRECTION('',(0.,-0.441506178461457,0.89725820942489));
#18789=DIRECTION('center_axis',(0.,-0.0645326704573515,-0.997915594849406));
#18790=DIRECTION('ref_axis',(-1.,0.,0.));
#18791=DIRECTION('',(0.,-0.997915594849406,0.0645326704573514));
#18792=DIRECTION('',(1.,0.,0.));
#18793=DIRECTION('center_axis',(0.,-0.660001395281353,-0.751264373058291));
#18794=DIRECTION('ref_axis',(-1.,0.,0.));
#18795=DIRECTION('',(-1.,0.,0.));
#18796=DIRECTION('',(0.,-0.751264373058291,0.660001395281353));
#18797=DIRECTION('center_axis',(0.,0.322265351633779,-0.946649377085496));
#18798=DIRECTION('ref_axis',(-1.,0.,0.));
#18799=DIRECTION('',(0.,-0.946649377085496,-0.322265351633779));
#18800=DIRECTION('',(1.,0.,0.));
#18801=DIRECTION('center_axis',(0.,-0.322265351633779,-0.946649377085496));
#18802=DIRECTION('ref_axis',(-1.,0.,0.));
#18803=DIRECTION('',(-1.,0.,0.));
#18804=DIRECTION('',(0.,-0.946649377085496,0.322265351633779));
#18805=DIRECTION('center_axis',(0.,0.660001395281352,-0.751264373058292));
#18806=DIRECTION('ref_axis',(-1.,0.,0.));
#18807=DIRECTION('',(0.,-0.751264373058292,-0.660001395281352));
#18808=DIRECTION('',(1.,0.,0.));
#18809=DIRECTION('center_axis',(0.,0.0645326704573514,-0.997915594849406));
#18810=DIRECTION('ref_axis',(-1.,0.,0.));
#18811=DIRECTION('',(-1.,0.,0.));
#18812=DIRECTION('',(0.,-0.997915594849406,-0.0645326704573514));
#18813=DIRECTION('center_axis',(0.,0.897258209424887,-0.441506178461464));
#18814=DIRECTION('ref_axis',(0.,0.441506178461464,0.897258209424887));
#18815=DIRECTION('',(0.,-0.441506178461464,-0.897258209424887));
#18816=DIRECTION('',(1.,0.,0.));
#18817=DIRECTION('center_axis',(0.,0.441506178461463,-0.897258209424887));
#18818=DIRECTION('ref_axis',(-1.,0.,0.));
#18819=DIRECTION('',(-1.,0.,0.));
#18820=DIRECTION('',(0.,-0.897258209424887,-0.441506178461463));
#18821=DIRECTION('center_axis',(0.,0.751264373058291,-0.660001395281353));
#18822=DIRECTION('ref_axis',(-1.,0.,0.));
#18823=DIRECTION('',(-1.,0.,0.));
#18824=DIRECTION('',(0.,-0.660001395281353,-0.751264373058291));
#18825=DIRECTION('center_axis',(0.,0.997915594849406,-0.0645326704573515));
#18826=DIRECTION('ref_axis',(0.,0.0645326704573514,0.997915594849406));
#18827=DIRECTION('',(0.,-0.0645326704573514,-0.997915594849406));
#18828=DIRECTION('',(1.,0.,0.));
#18829=DIRECTION('center_axis',(1.,0.,0.));
#18830=DIRECTION('ref_axis',(0.,-0.38268343236509,-0.923879532511287));
#18831=DIRECTION('center_axis',(1.,0.,0.));
#18832=DIRECTION('ref_axis',(0.,-0.38268343236509,-0.923879532511287));
#18833=DIRECTION('center_axis',(-1.,0.,0.));
#18834=DIRECTION('ref_axis',(0.,1.,0.));
#18835=DIRECTION('',(-0.707106781186548,-0.707106781186547,-8.65956056235493E-17));
#18836=DIRECTION('center_axis',(-1.,0.,0.));
#18837=DIRECTION('ref_axis',(0.,1.,0.));
#18838=DIRECTION('center_axis',(1.,0.,0.));
#18839=DIRECTION('ref_axis',(0.,0.,-1.));
#18840=DIRECTION('',(0.,4.06259722475401E-16,1.));
#18841=DIRECTION('',(0.,0.866025403784439,0.5));
#18842=DIRECTION('',(0.,0.866025403784439,-0.5));
#18843=DIRECTION('',(0.,1.354199074918E-16,-1.));
#18844=DIRECTION('',(0.,-0.866025403784439,-0.5));
#18845=DIRECTION('',(0.,-0.866025403784439,0.5));
#18846=DIRECTION('center_axis',(-0.707106781186548,0.353553390593274,-0.612372435695794));
#18847=DIRECTION('ref_axis',(-0.654653670707977,0.,0.755928946018455));
#18848=DIRECTION('',(0.,0.866025403784439,0.5));
#18849=DIRECTION('',(0.654653670707977,2.78478589689825E-15,-0.755928946018455));
#18850=DIRECTION('',(0.,-0.866025403784439,-0.5));
#18851=DIRECTION('',(0.654653670707977,0.654653670707979,-0.377964473009225));
#18852=DIRECTION('center_axis',(-0.707106781186547,-0.353553390593274,-0.612372435695795));
#18853=DIRECTION('ref_axis',(-0.654653670707977,0.,0.755928946018454));
#18854=DIRECTION('',(0.,0.866025403784439,-0.5));
#18855=DIRECTION('',(0.654653670707977,-0.654653670707978,-0.377964473009226));
#18856=DIRECTION('',(0.,-0.866025403784439,0.5));
#18857=DIRECTION('center_axis',(-0.707106781186547,-0.353553390593274,0.612372435695795));
#18858=DIRECTION('ref_axis',(0.654653670707978,0.,0.755928946018454));
#18859=DIRECTION('',(0.,-0.866025403784439,-0.5));
#18860=DIRECTION('',(0.654653670707976,5.13140401744201E-15,0.755928946018455));
#18861=DIRECTION('',(0.,0.866025403784439,0.5));
#18862=DIRECTION('',(-0.654653670707977,0.654653670707978,-0.377964473009226));
#18863=DIRECTION('center_axis',(-0.70710678118655,0.353553390593273,0.612372435695792));
#18864=DIRECTION('ref_axis',(0.654653670707975,0.,0.755928946018457));
#18865=DIRECTION('',(0.,0.866025403784439,-0.5));
#18866=DIRECTION('',(0.,-0.866025403784439,0.5));
#18867=DIRECTION('',(0.654653670707976,0.654653670707978,0.377964473009228));
#18868=DIRECTION('center_axis',(-0.707106781186548,-0.707106781186547,2.87269004685321E-16));
#18869=DIRECTION('ref_axis',(4.062597224754E-16,0.,1.));
#18870=DIRECTION('',(0.,-4.06259722475401E-16,-1.));
#18871=DIRECTION('',(0.,4.06259722475401E-16,1.));
#18872=DIRECTION('center_axis',(-0.707106781186548,0.707106781186547,9.57563348951068E-17));
#18873=DIRECTION('ref_axis',(1.354199074918E-16,0.,1.));
#18874=DIRECTION('',(0.,1.354199074918E-16,-1.));
#18875=DIRECTION('',(0.,-1.354199074918E-16,1.));
#18876=DIRECTION('center_axis',(0.,0.5,0.866025403784439));
#18877=DIRECTION('ref_axis',(0.,-0.866025403784439,0.5));
#18878=DIRECTION('',(1.,0.,0.));
#18879=DIRECTION('',(1.,0.,0.));
#18880=DIRECTION('center_axis',(0.,1.,-4.06259722475401E-16));
#18881=DIRECTION('ref_axis',(0.,4.06259722475401E-16,1.));
#18882=DIRECTION('',(1.,0.,0.));
#18883=DIRECTION('center_axis',(0.,0.5,-0.866025403784439));
#18884=DIRECTION('ref_axis',(0.,0.866025403784439,0.5));
#18885=DIRECTION('',(1.,0.,0.));
#18886=DIRECTION('center_axis',(-1.,0.,0.));
#18887=DIRECTION('ref_axis',(0.,0.,1.));
#18888=DIRECTION('center_axis',(1.,0.,0.));
#18889=DIRECTION('ref_axis',(0.,0.,-1.));
#18890=DIRECTION('center_axis',(0.,-0.5,-0.866025403784439));
#18891=DIRECTION('ref_axis',(0.,0.866025403784439,-0.5));
#18892=DIRECTION('',(1.,0.,0.));
#18893=DIRECTION('center_axis',(0.,-1.,-1.354199074918E-16));
#18894=DIRECTION('ref_axis',(0.,1.354199074918E-16,-1.));
#18895=DIRECTION('',(1.,0.,0.));
#18896=DIRECTION('center_axis',(0.,-0.5,0.866025403784439));
#18897=DIRECTION('ref_axis',(0.,-0.866025403784439,-0.5));
#18898=DIRECTION('center_axis',(1.,0.,0.));
#18899=DIRECTION('ref_axis',(0.,-0.38268343236509,-0.923879532511286));
#18900=DIRECTION('center_axis',(1.,0.,0.));
#18901=DIRECTION('ref_axis',(0.,-0.707106781186548,-0.707106781186547));
#18902=DIRECTION('center_axis',(1.,0.,0.));
#18903=DIRECTION('ref_axis',(0.,-0.707106781186548,-0.707106781186547));
#18904=DIRECTION('center_axis',(1.,0.,0.));
#18905=DIRECTION('ref_axis',(0.,-0.707106781186548,-0.707106781186547));
#18906=DIRECTION('center_axis',(1.,0.,0.));
#18907=DIRECTION('ref_axis',(0.,-0.923879532511287,-0.38268343236509));
#18908=DIRECTION('center_axis',(1.,0.,0.));
#18909=DIRECTION('ref_axis',(0.,-0.923879532511287,-0.38268343236509));
#18910=DIRECTION('center_axis',(1.,0.,0.));
#18911=DIRECTION('ref_axis',(0.,-0.923879532511287,-0.38268343236509));
#18912=DIRECTION('center_axis',(1.,0.,0.));
#18913=DIRECTION('ref_axis',(0.,-1.,1.83697019872103E-16));
#18914=DIRECTION('center_axis',(1.,0.,0.));
#18915=DIRECTION('ref_axis',(0.,-1.,1.83697019872103E-16));
#18916=DIRECTION('center_axis',(1.,0.,0.));
#18917=DIRECTION('ref_axis',(0.,-1.,1.83697019872103E-16));
#18918=DIRECTION('center_axis',(1.,0.,0.));
#18919=DIRECTION('ref_axis',(0.,-0.923879532511286,0.38268343236509));
#18920=DIRECTION('center_axis',(1.,0.,0.));
#18921=DIRECTION('ref_axis',(0.,-0.923879532511287,0.38268343236509));
#18922=DIRECTION('center_axis',(1.,0.,0.));
#18923=DIRECTION('ref_axis',(0.,-0.923879532511287,0.38268343236509));
#18924=DIRECTION('center_axis',(1.,0.,0.));
#18925=DIRECTION('ref_axis',(0.,-0.707106781186547,0.707106781186548));
#18926=DIRECTION('center_axis',(1.,0.,0.));
#18927=DIRECTION('ref_axis',(0.,-0.707106781186547,0.707106781186548));
#18928=DIRECTION('center_axis',(1.,0.,0.));
#18929=DIRECTION('ref_axis',(0.,-0.707106781186547,0.707106781186548));
#18930=DIRECTION('center_axis',(1.,0.,0.));
#18931=DIRECTION('ref_axis',(0.,-0.38268343236509,0.923879532511287));
#18932=DIRECTION('center_axis',(1.,0.,0.));
#18933=DIRECTION('ref_axis',(0.,-0.38268343236509,0.923879532511287));
#18934=DIRECTION('center_axis',(1.,0.,0.));
#18935=DIRECTION('ref_axis',(0.,-0.38268343236509,0.923879532511287));
#18936=DIRECTION('center_axis',(1.,0.,0.));
#18937=DIRECTION('ref_axis',(0.,1.22464679914735E-16,1.));
#18938=DIRECTION('center_axis',(1.,0.,0.));
#18939=DIRECTION('ref_axis',(0.,1.22464679914735E-16,1.));
#18940=DIRECTION('center_axis',(1.,0.,0.));
#18941=DIRECTION('ref_axis',(0.,1.22464679914735E-16,1.));
#18942=DIRECTION('center_axis',(1.,0.,0.));
#18943=DIRECTION('ref_axis',(0.,0.38268343236509,0.923879532511287));
#18944=DIRECTION('center_axis',(1.,0.,0.));
#18945=DIRECTION('ref_axis',(0.,0.38268343236509,0.923879532511287));
#18946=DIRECTION('center_axis',(1.,0.,0.));
#18947=DIRECTION('ref_axis',(0.,0.38268343236509,0.923879532511287));
#18948=DIRECTION('center_axis',(1.,0.,0.));
#18949=DIRECTION('ref_axis',(0.,0.707106781186548,0.707106781186547));
#18950=DIRECTION('center_axis',(1.,0.,0.));
#18951=DIRECTION('ref_axis',(0.,0.707106781186548,0.707106781186547));
#18952=DIRECTION('center_axis',(1.,0.,0.));
#18953=DIRECTION('ref_axis',(0.,0.707106781186548,0.707106781186547));
#18954=DIRECTION('center_axis',(1.,0.,0.));
#18955=DIRECTION('ref_axis',(0.,0.923879532511287,0.38268343236509));
#18956=DIRECTION('center_axis',(1.,0.,0.));
#18957=DIRECTION('ref_axis',(0.,0.923879532511287,0.38268343236509));
#18958=DIRECTION('center_axis',(1.,0.,0.));
#18959=DIRECTION('ref_axis',(0.,0.923879532511287,0.38268343236509));
#18960=DIRECTION('center_axis',(1.,0.,0.));
#18961=DIRECTION('ref_axis',(0.,1.,-6.12323399573677E-17));
#18962=DIRECTION('center_axis',(1.,0.,0.));
#18963=DIRECTION('ref_axis',(0.,1.,-6.12323399573677E-17));
#18964=DIRECTION('center_axis',(1.,0.,0.));
#18965=DIRECTION('ref_axis',(0.,1.,-6.12323399573677E-17));
#18966=DIRECTION('center_axis',(1.,0.,0.));
#18967=DIRECTION('ref_axis',(0.,0.923879532511287,-0.38268343236509));
#18968=DIRECTION('center_axis',(1.,0.,0.));
#18969=DIRECTION('ref_axis',(0.,0.923879532511287,-0.38268343236509));
#18970=DIRECTION('center_axis',(1.,0.,0.));
#18971=DIRECTION('ref_axis',(0.,0.923879532511287,-0.38268343236509));
#18972=DIRECTION('center_axis',(1.,0.,0.));
#18973=DIRECTION('ref_axis',(0.,0.707106781186548,-0.707106781186548));
#18974=DIRECTION('center_axis',(1.,0.,0.));
#18975=DIRECTION('ref_axis',(0.,0.707106781186548,-0.707106781186548));
#18976=DIRECTION('center_axis',(1.,0.,0.));
#18977=DIRECTION('ref_axis',(0.,0.707106781186548,-0.707106781186548));
#18978=DIRECTION('center_axis',(1.,0.,0.));
#18979=DIRECTION('ref_axis',(0.,0.38268343236509,-0.923879532511287));
#18980=DIRECTION('center_axis',(1.,0.,0.));
#18981=DIRECTION('ref_axis',(0.,0.38268343236509,-0.923879532511287));
#18982=DIRECTION('center_axis',(1.,0.,0.));
#18983=DIRECTION('ref_axis',(0.,0.38268343236509,-0.923879532511287));
#18984=DIRECTION('center_axis',(1.,0.,0.));
#18985=DIRECTION('ref_axis',(0.,0.,-1.));
#18986=DIRECTION('center_axis',(1.,0.,0.));
#18987=DIRECTION('ref_axis',(0.,0.,-1.));
#18988=DIRECTION('center_axis',(1.,0.,0.));
#18989=DIRECTION('ref_axis',(0.,0.,-1.));
#18990=DIRECTION('center_axis',(1.,0.,0.));
#18991=DIRECTION('ref_axis',(0.,1.,0.));
#18992=DIRECTION('',(-0.707106781186547,0.707106781186548,8.65956056235494E-17));
#18993=DIRECTION('axis',(0.,0.,1.));
#18994=DIRECTION('refdir',(1.,0.,0.));
#18995=DIRECTION('center_axis',(1.,0.,0.));
#18996=DIRECTION('ref_axis',(0.,1.,0.));
#18997=DIRECTION('',(-1.,0.,0.));
#18998=DIRECTION('center_axis',(1.,0.,0.));
#18999=DIRECTION('ref_axis',(0.,1.,0.));
#19000=DIRECTION('center_axis',(1.,0.,0.));
#19001=DIRECTION('ref_axis',(0.,1.,0.));
#19002=DIRECTION('',(-1.,0.,0.));
#19003=DIRECTION('center_axis',(1.,0.,0.));
#19004=DIRECTION('ref_axis',(0.,1.,0.));
#19005=DIRECTION('',(-1.,0.,0.));
#19006=DIRECTION('center_axis',(1.,0.,0.));
#19007=DIRECTION('ref_axis',(0.,1.,0.));
#19008=DIRECTION('',(-1.,0.,0.));
#19009=DIRECTION('center_axis',(1.,0.,0.));
#19010=DIRECTION('ref_axis',(0.,1.,0.));
#19011=DIRECTION('',(-1.,0.,0.));
#19012=DIRECTION('center_axis',(1.,0.,0.));
#19013=DIRECTION('ref_axis',(0.,1.,0.));
#19014=DIRECTION('',(-1.,0.,0.));
#19015=DIRECTION('center_axis',(1.,0.,0.));
#19016=DIRECTION('ref_axis',(0.,1.,0.));
#19017=DIRECTION('',(-1.,0.,0.));
#19018=DIRECTION('center_axis',(1.,0.,0.));
#19019=DIRECTION('ref_axis',(0.,1.,0.));
#19020=DIRECTION('',(-1.,0.,0.));
#19021=DIRECTION('center_axis',(1.,0.,0.));
#19022=DIRECTION('ref_axis',(0.,1.,0.));
#19023=DIRECTION('',(-1.,0.,0.));
#19024=DIRECTION('center_axis',(1.,0.,0.));
#19025=DIRECTION('ref_axis',(0.,1.,0.));
#19026=DIRECTION('',(-1.,0.,0.));
#19027=DIRECTION('center_axis',(1.,0.,0.));
#19028=DIRECTION('ref_axis',(0.,1.,0.));
#19029=DIRECTION('',(-1.,0.,0.));
#19030=DIRECTION('center_axis',(1.,0.,0.));
#19031=DIRECTION('ref_axis',(0.,1.,0.));
#19032=DIRECTION('',(-1.,0.,0.));
#19033=DIRECTION('center_axis',(1.,0.,0.));
#19034=DIRECTION('ref_axis',(0.,1.,0.));
#19035=DIRECTION('',(-1.,0.,0.));
#19036=DIRECTION('center_axis',(1.,0.,0.));
#19037=DIRECTION('ref_axis',(0.,1.,0.));
#19038=DIRECTION('',(-1.,0.,0.));
#19039=DIRECTION('center_axis',(1.,0.,0.));
#19040=DIRECTION('ref_axis',(0.,1.,0.));
#19041=DIRECTION('',(-1.,0.,0.));
#19042=DIRECTION('center_axis',(1.,0.,0.));
#19043=DIRECTION('ref_axis',(0.,1.,0.));
#19044=DIRECTION('',(-1.,0.,0.));
#19045=DIRECTION('center_axis',(1.,0.,0.));
#19046=DIRECTION('ref_axis',(0.,1.,0.));
#19047=DIRECTION('',(-1.,0.,0.));
#19048=DIRECTION('center_axis',(1.,0.,0.));
#19049=DIRECTION('ref_axis',(0.,1.,0.));
#19050=DIRECTION('',(-1.,0.,0.));
#19051=DIRECTION('center_axis',(1.,0.,0.));
#19052=DIRECTION('ref_axis',(0.,1.,0.));
#19053=DIRECTION('',(-1.,0.,0.));
#19054=DIRECTION('center_axis',(1.,0.,0.));
#19055=DIRECTION('ref_axis',(0.,1.,0.));
#19056=DIRECTION('',(-1.,0.,0.));
#19057=DIRECTION('center_axis',(1.,0.,0.));
#19058=DIRECTION('ref_axis',(0.,1.,0.));
#19059=DIRECTION('',(-1.,0.,0.));
#19060=DIRECTION('center_axis',(1.,0.,0.));
#19061=DIRECTION('ref_axis',(0.,1.,0.));
#19062=DIRECTION('',(-1.,0.,0.));
#19063=DIRECTION('center_axis',(1.,0.,0.));
#19064=DIRECTION('ref_axis',(0.,1.,0.));
#19065=DIRECTION('',(-1.,0.,0.));
#19066=DIRECTION('center_axis',(1.,0.,0.));
#19067=DIRECTION('ref_axis',(0.,1.,4.93993055488555E-14));
#19068=DIRECTION('',(1.,0.,0.));
#19069=DIRECTION('center_axis',(1.,0.,0.));
#19070=DIRECTION('ref_axis',(0.,1.,4.93993055488555E-14));
#19071=DIRECTION('center_axis',(1.,0.,0.));
#19072=DIRECTION('ref_axis',(0.,1.,4.93993055488555E-14));
#19073=DIRECTION('',(1.,0.,0.));
#19074=DIRECTION('center_axis',(1.,0.,0.));
#19075=DIRECTION('ref_axis',(0.,1.,4.93993055488555E-14));
#19076=DIRECTION('',(1.,0.,0.));
#19077=DIRECTION('center_axis',(1.,0.,0.));
#19078=DIRECTION('ref_axis',(0.,1.,4.93993055488555E-14));
#19079=DIRECTION('',(1.,0.,0.));
#19080=DIRECTION('center_axis',(1.,0.,0.));
#19081=DIRECTION('ref_axis',(0.,1.,4.93993055488555E-14));
#19082=DIRECTION('',(1.,0.,0.));
#19083=DIRECTION('center_axis',(1.,0.,0.));
#19084=DIRECTION('ref_axis',(0.,1.,4.93993055488555E-14));
#19085=DIRECTION('',(1.,0.,0.));
#19086=DIRECTION('center_axis',(1.,0.,0.));
#19087=DIRECTION('ref_axis',(0.,1.,4.93993055488555E-14));
#19088=DIRECTION('',(1.,0.,0.));
#19089=DIRECTION('center_axis',(1.,0.,0.));
#19090=DIRECTION('ref_axis',(0.,1.,4.93993055488555E-14));
#19091=DIRECTION('',(1.,0.,0.));
#19092=DIRECTION('center_axis',(1.,0.,0.));
#19093=DIRECTION('ref_axis',(0.,1.,4.93993055488555E-14));
#19094=DIRECTION('',(1.,0.,0.));
#19095=DIRECTION('center_axis',(1.,0.,0.));
#19096=DIRECTION('ref_axis',(0.,1.,4.93993055488555E-14));
#19097=DIRECTION('',(1.,0.,0.));
#19098=DIRECTION('center_axis',(1.,0.,0.));
#19099=DIRECTION('ref_axis',(0.,1.,4.93993055488555E-14));
#19100=DIRECTION('',(1.,0.,0.));
#19101=DIRECTION('center_axis',(1.,0.,0.));
#19102=DIRECTION('ref_axis',(0.,1.,4.93993055488555E-14));
#19103=DIRECTION('',(1.,0.,0.));
#19104=DIRECTION('center_axis',(1.,0.,0.));
#19105=DIRECTION('ref_axis',(0.,1.,4.93993055488555E-14));
#19106=DIRECTION('',(1.,0.,0.));
#19107=DIRECTION('center_axis',(1.,0.,0.));
#19108=DIRECTION('ref_axis',(0.,1.,4.93993055488555E-14));
#19109=DIRECTION('',(1.,0.,0.));
#19110=DIRECTION('center_axis',(1.,0.,0.));
#19111=DIRECTION('ref_axis',(0.,1.,4.93993055488555E-14));
#19112=DIRECTION('',(1.,0.,0.));
#19113=DIRECTION('center_axis',(1.,0.,0.));
#19114=DIRECTION('ref_axis',(0.,1.,4.93993055488555E-14));
#19115=DIRECTION('',(1.,0.,0.));
#19116=DIRECTION('center_axis',(1.,0.,0.));
#19117=DIRECTION('ref_axis',(0.,1.,4.93993055488555E-14));
#19118=DIRECTION('',(1.,0.,0.));
#19119=DIRECTION('center_axis',(1.,0.,0.));
#19120=DIRECTION('ref_axis',(0.,1.,4.93993055488555E-14));
#19121=DIRECTION('',(1.,0.,0.));
#19122=DIRECTION('center_axis',(1.,0.,0.));
#19123=DIRECTION('ref_axis',(0.,1.,4.93993055488555E-14));
#19124=DIRECTION('',(1.,0.,0.));
#19125=DIRECTION('center_axis',(1.,0.,0.));
#19126=DIRECTION('ref_axis',(0.,1.,4.93993055488555E-14));
#19127=DIRECTION('',(1.,0.,0.));
#19128=DIRECTION('center_axis',(1.,0.,0.));
#19129=DIRECTION('ref_axis',(0.,1.,4.93993055488555E-14));
#19130=DIRECTION('',(1.,0.,0.));
#19131=DIRECTION('center_axis',(1.,0.,0.));
#19132=DIRECTION('ref_axis',(0.,1.,4.93993055488555E-14));
#19133=DIRECTION('',(1.,0.,0.));
#19134=DIRECTION('center_axis',(1.,0.,0.));
#19135=DIRECTION('ref_axis',(0.,0.,-1.));
#19136=DIRECTION('center_axis',(1.,0.,0.));
#19137=DIRECTION('ref_axis',(0.,1.,0.));
#19138=DIRECTION('center_axis',(1.,0.,0.));
#19139=DIRECTION('ref_axis',(0.,1.,0.));
#19140=DIRECTION('center_axis',(-1.,0.,0.));
#19141=DIRECTION('ref_axis',(0.,1.,4.93993055488555E-14));
#19142=DIRECTION('center_axis',(1.,0.,0.));
#19143=DIRECTION('ref_axis',(0.,1.,4.93993055488555E-14));
#19144=DIRECTION('center_axis',(1.,0.,0.));
#19145=DIRECTION('ref_axis',(0.,1.,0.));
#19146=DIRECTION('center_axis',(-1.,0.,0.));
#19147=DIRECTION('ref_axis',(0.,1.,0.));
#19148=DIRECTION('center_axis',(-1.,0.,0.));
#19149=DIRECTION('ref_axis',(0.,0.,1.));
#19150=DIRECTION('center_axis',(1.,0.,0.));
#19151=DIRECTION('ref_axis',(0.,0.,-1.));
#19152=DIRECTION('center_axis',(1.,0.,0.));
#19153=DIRECTION('ref_axis',(0.,1.,0.));
#19154=DIRECTION('',(-0.707106781186548,0.707106781186547,8.65956056235493E-17));
#19155=DIRECTION('center_axis',(-1.,0.,0.));
#19156=DIRECTION('ref_axis',(0.,1.,0.));
#19157=DIRECTION('',(0.506349288588207,0.862328474507375,1.05604780611908E-16));
#19158=DIRECTION('center_axis',(1.,0.,0.));
#19159=DIRECTION('ref_axis',(0.,1.,0.));
#19160=DIRECTION('center_axis',(0.,-0.5,0.866025403784439));
#19161=DIRECTION('ref_axis',(0.,-0.866025403784439,-0.5));
#19162=DIRECTION('',(1.,0.,0.));
#19163=DIRECTION('',(0.,-0.866025403784439,-0.5));
#19164=DIRECTION('',(1.,0.,0.));
#19165=DIRECTION('center_axis',(0.,0.5,0.866025403784439));
#19166=DIRECTION('ref_axis',(0.,-0.866025403784439,0.5));
#19167=DIRECTION('',(1.,0.,0.));
#19168=DIRECTION('',(0.,-0.866025403784439,0.5));
#19169=DIRECTION('center_axis',(0.,1.,-2.74708955197652E-16));
#19170=DIRECTION('ref_axis',(0.,2.74708955197652E-16,1.));
#19171=DIRECTION('',(1.,0.,0.));
#19172=DIRECTION('',(0.,2.74708955197652E-16,1.));
#19173=DIRECTION('center_axis',(0.,0.5,-0.866025403784439));
#19174=DIRECTION('ref_axis',(0.,0.866025403784439,0.5));
#19175=DIRECTION('',(1.,0.,0.));
#19176=DIRECTION('',(0.,0.866025403784439,0.5));
#19177=DIRECTION('center_axis',(0.,-0.5,-0.866025403784439));
#19178=DIRECTION('ref_axis',(0.,0.866025403784439,-0.5));
#19179=DIRECTION('',(1.,0.,0.));
#19180=DIRECTION('',(0.,0.866025403784439,-0.5));
#19181=DIRECTION('center_axis',(0.,-1.,-1.37354477598826E-16));
#19182=DIRECTION('ref_axis',(0.,1.37354477598826E-16,-1.));
#19183=DIRECTION('',(0.,1.37354477598826E-16,-1.));
#19184=DIRECTION('center_axis',(1.,0.,0.));
#19185=DIRECTION('ref_axis',(0.,0.,-1.));
#19186=DIRECTION('center_axis',(1.,0.,0.));
#19187=DIRECTION('ref_axis',(0.,0.,-1.));
#19188=DIRECTION('axis',(0.,0.,1.));
#19189=DIRECTION('refdir',(1.,0.,0.));
#19190=DIRECTION('center_axis',(1.,0.,0.));
#19191=DIRECTION('ref_axis',(0.,1.,0.));
#19192=DIRECTION('',(-1.,0.,0.));
#19193=DIRECTION('center_axis',(1.,0.,0.));
#19194=DIRECTION('ref_axis',(0.,1.,0.));
#19195=DIRECTION('center_axis',(1.,0.,0.));
#19196=DIRECTION('ref_axis',(0.,1.,0.));
#19197=DIRECTION('',(-1.,0.,0.));
#19198=DIRECTION('center_axis',(1.,0.,0.));
#19199=DIRECTION('ref_axis',(0.,1.,0.));
#19200=DIRECTION('',(-1.,0.,0.));
#19201=DIRECTION('center_axis',(1.,0.,0.));
#19202=DIRECTION('ref_axis',(0.,1.,0.));
#19203=DIRECTION('',(-1.,0.,0.));
#19204=DIRECTION('center_axis',(1.,0.,0.));
#19205=DIRECTION('ref_axis',(0.,1.,0.));
#19206=DIRECTION('',(-1.,0.,0.));
#19207=DIRECTION('center_axis',(1.,0.,0.));
#19208=DIRECTION('ref_axis',(0.,1.,0.));
#19209=DIRECTION('',(-1.,0.,0.));
#19210=DIRECTION('center_axis',(1.,0.,0.));
#19211=DIRECTION('ref_axis',(0.,1.,0.));
#19212=DIRECTION('',(-1.,0.,0.));
#19213=DIRECTION('center_axis',(1.,0.,0.));
#19214=DIRECTION('ref_axis',(0.,1.,0.));
#19215=DIRECTION('',(-1.,0.,0.));
#19216=DIRECTION('center_axis',(1.,0.,0.));
#19217=DIRECTION('ref_axis',(0.,1.,0.));
#19218=DIRECTION('',(-1.,0.,0.));
#19219=DIRECTION('center_axis',(1.,0.,0.));
#19220=DIRECTION('ref_axis',(0.,1.,0.));
#19221=DIRECTION('',(-1.,0.,0.));
#19222=DIRECTION('center_axis',(1.,0.,0.));
#19223=DIRECTION('ref_axis',(0.,1.,0.));
#19224=DIRECTION('',(-1.,0.,0.));
#19225=DIRECTION('center_axis',(1.,0.,0.));
#19226=DIRECTION('ref_axis',(0.,1.,0.));
#19227=DIRECTION('',(-1.,0.,0.));
#19228=DIRECTION('center_axis',(1.,0.,0.));
#19229=DIRECTION('ref_axis',(0.,1.,0.));
#19230=DIRECTION('',(-1.,0.,0.));
#19231=DIRECTION('center_axis',(1.,0.,0.));
#19232=DIRECTION('ref_axis',(0.,1.,0.));
#19233=DIRECTION('',(-1.,0.,0.));
#19234=DIRECTION('center_axis',(1.,0.,0.));
#19235=DIRECTION('ref_axis',(0.,1.,0.));
#19236=DIRECTION('',(-1.,0.,0.));
#19237=DIRECTION('center_axis',(1.,0.,0.));
#19238=DIRECTION('ref_axis',(0.,1.,0.));
#19239=DIRECTION('',(-1.,0.,0.));
#19240=DIRECTION('center_axis',(1.,0.,0.));
#19241=DIRECTION('ref_axis',(0.,1.,0.));
#19242=DIRECTION('',(-1.,0.,0.));
#19243=DIRECTION('center_axis',(1.,0.,0.));
#19244=DIRECTION('ref_axis',(0.,1.,0.));
#19245=DIRECTION('',(-1.,0.,0.));
#19246=DIRECTION('center_axis',(1.,0.,0.));
#19247=DIRECTION('ref_axis',(0.,1.,0.));
#19248=DIRECTION('',(-1.,0.,0.));
#19249=DIRECTION('center_axis',(1.,0.,0.));
#19250=DIRECTION('ref_axis',(0.,1.,0.));
#19251=DIRECTION('',(-1.,0.,0.));
#19252=DIRECTION('center_axis',(1.,0.,0.));
#19253=DIRECTION('ref_axis',(0.,1.,0.));
#19254=DIRECTION('',(-1.,0.,0.));
#19255=DIRECTION('center_axis',(1.,0.,0.));
#19256=DIRECTION('ref_axis',(0.,1.,0.));
#19257=DIRECTION('',(-1.,0.,0.));
#19258=DIRECTION('center_axis',(1.,0.,0.));
#19259=DIRECTION('ref_axis',(0.,1.,0.));
#19260=DIRECTION('',(-1.,0.,0.));
#19261=DIRECTION('center_axis',(1.,0.,0.));
#19262=DIRECTION('ref_axis',(0.,1.,0.));
#19263=DIRECTION('',(-1.,0.,0.));
#19264=DIRECTION('center_axis',(1.,0.,0.));
#19265=DIRECTION('ref_axis',(0.,1.,0.));
#19266=DIRECTION('',(-1.,0.,0.));
#19267=DIRECTION('center_axis',(1.,0.,0.));
#19268=DIRECTION('ref_axis',(0.,1.,0.));
#19269=DIRECTION('',(-1.,0.,0.));
#19270=DIRECTION('center_axis',(1.,0.,0.));
#19271=DIRECTION('ref_axis',(0.,1.,0.));
#19272=DIRECTION('',(-1.,0.,0.));
#19273=DIRECTION('center_axis',(1.,0.,0.));
#19274=DIRECTION('ref_axis',(0.,1.,0.));
#19275=DIRECTION('',(-1.,0.,0.));
#19276=DIRECTION('center_axis',(1.,0.,0.));
#19277=DIRECTION('ref_axis',(0.,-0.266010182744204,-0.963970218770474));
#19278=DIRECTION('',(1.,0.,0.));
#19279=DIRECTION('center_axis',(1.,0.,0.));
#19280=DIRECTION('ref_axis',(0.,1.,-1.17958518182489E-13));
#19281=DIRECTION('center_axis',(1.,0.,0.));
#19282=DIRECTION('ref_axis',(0.,1.,-1.17958518182489E-13));
#19283=DIRECTION('',(1.,0.,0.));
#19284=DIRECTION('center_axis',(1.,0.,0.));
#19285=DIRECTION('ref_axis',(0.,1.,-1.17958518182489E-13));
#19286=DIRECTION('',(1.,0.,0.));
#19287=DIRECTION('center_axis',(1.,0.,0.));
#19288=DIRECTION('ref_axis',(0.,1.,-1.17958518182489E-13));
#19289=DIRECTION('',(1.,0.,0.));
#19290=DIRECTION('center_axis',(1.,0.,0.));
#19291=DIRECTION('ref_axis',(0.,1.,-1.17958518182489E-13));
#19292=DIRECTION('',(1.,0.,0.));
#19293=DIRECTION('center_axis',(1.,0.,0.));
#19294=DIRECTION('ref_axis',(0.,1.,-1.17958518182489E-13));
#19295=DIRECTION('',(1.,0.,0.));
#19296=DIRECTION('center_axis',(1.,0.,0.));
#19297=DIRECTION('ref_axis',(0.,1.,-1.17958518182489E-13));
#19298=DIRECTION('',(1.,0.,0.));
#19299=DIRECTION('center_axis',(1.,0.,0.));
#19300=DIRECTION('ref_axis',(0.,1.,-1.17958518182489E-13));
#19301=DIRECTION('',(1.,0.,0.));
#19302=DIRECTION('center_axis',(1.,0.,0.));
#19303=DIRECTION('ref_axis',(0.,1.,-1.17958518182489E-13));
#19304=DIRECTION('',(1.,0.,0.));
#19305=DIRECTION('center_axis',(1.,0.,0.));
#19306=DIRECTION('ref_axis',(0.,1.,-1.17958518182489E-13));
#19307=DIRECTION('',(1.,0.,0.));
#19308=DIRECTION('center_axis',(1.,0.,0.));
#19309=DIRECTION('ref_axis',(0.,1.,-1.17958518182489E-13));
#19310=DIRECTION('',(1.,0.,0.));
#19311=DIRECTION('center_axis',(1.,0.,0.));
#19312=DIRECTION('ref_axis',(0.,1.,-1.17958518182489E-13));
#19313=DIRECTION('',(1.,0.,0.));
#19314=DIRECTION('center_axis',(1.,0.,0.));
#19315=DIRECTION('ref_axis',(0.,1.,-1.17958518182489E-13));
#19316=DIRECTION('',(1.,0.,0.));
#19317=DIRECTION('center_axis',(1.,0.,0.));
#19318=DIRECTION('ref_axis',(0.,1.,-1.17958518182489E-13));
#19319=DIRECTION('',(1.,0.,0.));
#19320=DIRECTION('center_axis',(1.,0.,0.));
#19321=DIRECTION('ref_axis',(0.,1.,-1.17958518182489E-13));
#19322=DIRECTION('',(1.,0.,0.));
#19323=DIRECTION('center_axis',(1.,0.,0.));
#19324=DIRECTION('ref_axis',(0.,1.,-1.17958518182489E-13));
#19325=DIRECTION('',(1.,0.,0.));
#19326=DIRECTION('center_axis',(1.,0.,0.));
#19327=DIRECTION('ref_axis',(0.,1.,-1.17958518182489E-13));
#19328=DIRECTION('',(1.,0.,0.));
#19329=DIRECTION('center_axis',(1.,0.,0.));
#19330=DIRECTION('ref_axis',(0.,1.,-1.17958518182489E-13));
#19331=DIRECTION('',(1.,0.,0.));
#19332=DIRECTION('center_axis',(1.,0.,0.));
#19333=DIRECTION('ref_axis',(0.,1.,-1.17958518182489E-13));
#19334=DIRECTION('',(1.,0.,0.));
#19335=DIRECTION('center_axis',(1.,0.,0.));
#19336=DIRECTION('ref_axis',(0.,1.,-1.17958518182489E-13));
#19337=DIRECTION('',(1.,0.,0.));
#19338=DIRECTION('center_axis',(1.,0.,0.));
#19339=DIRECTION('ref_axis',(0.,1.,-1.17958518182489E-13));
#19340=DIRECTION('',(1.,0.,0.));
#19341=DIRECTION('center_axis',(1.,0.,0.));
#19342=DIRECTION('ref_axis',(0.,1.,-1.17958518182489E-13));
#19343=DIRECTION('',(1.,0.,0.));
#19344=DIRECTION('center_axis',(1.,0.,0.));
#19345=DIRECTION('ref_axis',(0.,1.,-1.17958518182489E-13));
#19346=DIRECTION('',(1.,0.,0.));
#19347=DIRECTION('center_axis',(1.,0.,0.));
#19348=DIRECTION('ref_axis',(0.,1.,-1.17958518182489E-13));
#19349=DIRECTION('',(1.,0.,0.));
#19350=DIRECTION('center_axis',(1.,0.,0.));
#19351=DIRECTION('ref_axis',(0.,1.,-1.17958518182489E-13));
#19352=DIRECTION('',(1.,0.,0.));
#19353=DIRECTION('center_axis',(1.,0.,0.));
#19354=DIRECTION('ref_axis',(0.,1.,-1.17958518182489E-13));
#19355=DIRECTION('',(1.,0.,0.));
#19356=DIRECTION('center_axis',(1.,0.,0.));
#19357=DIRECTION('ref_axis',(0.,1.,-1.17958518182489E-13));
#19358=DIRECTION('',(1.,0.,0.));
#19359=DIRECTION('center_axis',(1.,0.,0.));
#19360=DIRECTION('ref_axis',(0.,1.,-1.17958518182489E-13));
#19361=DIRECTION('',(1.,0.,0.));
#19362=DIRECTION('center_axis',(1.,0.,0.));
#19363=DIRECTION('ref_axis',(0.,0.,-1.));
#19364=DIRECTION('center_axis',(1.,0.,0.));
#19365=DIRECTION('ref_axis',(0.,1.,0.));
#19366=DIRECTION('center_axis',(1.,0.,0.));
#19367=DIRECTION('ref_axis',(0.,1.,0.));
#19368=DIRECTION('center_axis',(-1.,0.,0.));
#19369=DIRECTION('ref_axis',(0.,1.,-1.17958518182489E-13));
#19370=DIRECTION('center_axis',(1.,0.,0.));
#19371=DIRECTION('ref_axis',(0.,1.,-1.17958518182489E-13));
#19372=DIRECTION('center_axis',(1.,0.,0.));
#19373=DIRECTION('ref_axis',(0.,1.,0.));
#19374=DIRECTION('',(0.520049754552021,-0.854135968561436,-1.04601487993539E-16));
#19375=DIRECTION('center_axis',(-1.,0.,0.));
#19376=DIRECTION('ref_axis',(0.,1.,0.));
#19377=DIRECTION('center_axis',(0.,-0.5,-0.866025403784439));
#19378=DIRECTION('ref_axis',(0.,-0.866025403784439,0.5));
#19379=DIRECTION('',(-1.,0.,0.));
#19380=DIRECTION('',(0.,-0.866025403784439,0.5));
#19381=DIRECTION('',(-1.,0.,0.));
#19382=DIRECTION('center_axis',(0.,-1.,-1.92296268638356E-16));
#19383=DIRECTION('ref_axis',(0.,-1.92296268638356E-16,1.));
#19384=DIRECTION('',(0.,-1.92296268638356E-16,1.));
#19385=DIRECTION('',(-1.,0.,0.));
#19386=DIRECTION('center_axis',(0.,-0.5,0.866025403784439));
#19387=DIRECTION('ref_axis',(0.,0.866025403784439,0.5));
#19388=DIRECTION('',(0.,0.866025403784439,0.5));
#19389=DIRECTION('',(-1.,0.,0.));
#19390=DIRECTION('center_axis',(0.,0.5,0.866025403784439));
#19391=DIRECTION('ref_axis',(0.,0.866025403784439,-0.5));
#19392=DIRECTION('',(0.,0.866025403784439,-0.5));
#19393=DIRECTION('',(-1.,0.,0.));
#19394=DIRECTION('center_axis',(0.,0.5,-0.866025403784439));
#19395=DIRECTION('ref_axis',(0.,-0.866025403784439,-0.5));
#19396=DIRECTION('',(-1.,0.,0.));
#19397=DIRECTION('',(0.,-0.866025403784439,-0.5));
#19398=DIRECTION('center_axis',(0.,1.,-3.84592537276713E-16));
#19399=DIRECTION('ref_axis',(0.,-3.84592537276713E-16,-1.));
#19400=DIRECTION('',(0.,-3.84592537276713E-16,-1.));
#19401=DIRECTION('center_axis',(-1.,0.,0.));
#19402=DIRECTION('ref_axis',(0.,0.,1.));
#19403=DIRECTION('center_axis',(-1.,0.,0.));
#19404=DIRECTION('ref_axis',(0.,0.,1.));
#19405=DIRECTION('center_axis',(1.,0.,0.));
#19406=DIRECTION('ref_axis',(0.,0.,-1.));
#19407=DIRECTION('center_axis',(1.,0.,0.));
#19408=DIRECTION('ref_axis',(0.,1.,0.));
#19409=DIRECTION('',(-0.707106781186546,0.707106781186549,8.65956056235496E-17));
#19410=DIRECTION('center_axis',(1.,0.,0.));
#19411=DIRECTION('ref_axis',(0.,0.93907309915965,-0.343717492186083));
#19412=DIRECTION('center_axis',(1.,0.,0.));
#19413=DIRECTION('ref_axis',(0.,1.,0.));
#19414=DIRECTION('center_axis',(-1.,0.,0.));
#19415=DIRECTION('ref_axis',(0.,0.,1.));
#19416=DIRECTION('center_axis',(1.,0.,0.));
#19417=DIRECTION('ref_axis',(0.,0.,-1.));
#19418=DIRECTION('center_axis',(1.,0.,0.));
#19419=DIRECTION('ref_axis',(0.,1.,0.));
#19420=DIRECTION('center_axis',(1.,0.,0.));
#19421=DIRECTION('ref_axis',(0.,0.,-1.));
#19422=DIRECTION('',(-1.,0.,0.));
#19423=DIRECTION('center_axis',(1.,0.,0.));
#19424=DIRECTION('ref_axis',(0.,0.,-1.));
#19425=DIRECTION('axis',(0.,0.,1.));
#19426=DIRECTION('refdir',(1.,0.,0.));
#19427=DIRECTION('center_axis',(-1.,0.,0.));
#19428=DIRECTION('ref_axis',(0.,-1.,0.));
#19429=DIRECTION('center_axis',(-1.,0.,0.));
#19430=DIRECTION('ref_axis',(0.,-1.,0.));
#19431=DIRECTION('',(-0.707106781186547,0.707106781186548,8.65956056235494E-17));
#19432=DIRECTION('center_axis',(1.,0.,0.));
#19433=DIRECTION('ref_axis',(0.,-1.,0.));
#19434=DIRECTION('center_axis',(1.,0.,0.));
#19435=DIRECTION('ref_axis',(0.,-1.,0.));
#19436=DIRECTION('center_axis',(1.,0.,0.));
#19437=DIRECTION('ref_axis',(0.,1.,0.));
#19438=DIRECTION('',(-1.,0.,0.));
#19439=DIRECTION('center_axis',(1.,0.,0.));
#19440=DIRECTION('ref_axis',(0.,0.,-1.));
#19441=DIRECTION('center_axis',(1.,0.,0.));
#19442=DIRECTION('ref_axis',(0.,0.,-1.));
#19443=DIRECTION('center_axis',(1.,0.,0.));
#19444=DIRECTION('ref_axis',(0.,0.,-1.));
#19445=DIRECTION('center_axis',(1.,0.,0.));
#19446=DIRECTION('ref_axis',(0.,1.,0.));
#19447=DIRECTION('',(-1.,0.,0.));
#19448=DIRECTION('center_axis',(1.,0.,0.));
#19449=DIRECTION('ref_axis',(0.,0.,-1.));
#19450=DIRECTION('center_axis',(-1.,0.,0.));
#19451=DIRECTION('ref_axis',(0.,0.,1.));
#19452=DIRECTION('center_axis',(1.,0.,0.));
#19453=DIRECTION('ref_axis',(0.,0.,-1.));
#19454=DIRECTION('center_axis',(1.,0.,0.));
#19455=DIRECTION('ref_axis',(0.,1.,0.));
#19456=DIRECTION('',(-0.707106781186546,0.707106781186549,8.65956056235496E-17));
#19457=DIRECTION('axis',(0.,0.,1.));
#19458=DIRECTION('refdir',(1.,0.,0.));
#19459=DIRECTION('center_axis',(0.,0.866025403784439,0.5));
#19460=DIRECTION('ref_axis',(1.,0.,0.));
#19461=DIRECTION('',(-1.,0.,0.));
#19462=DIRECTION('',(1.,0.,0.));
#19463=DIRECTION('center_axis',(0.,1.,-2.74708955197652E-16));
#19464=DIRECTION('ref_axis',(0.,2.74708955197652E-16,1.));
#19465=DIRECTION('',(1.,0.,0.));
#19466=DIRECTION('center_axis',(-1.,0.,0.));
#19467=DIRECTION('ref_axis',(0.,1.,0.));
#19468=DIRECTION('',(0.506349288588207,0.862328474507375,1.05604780611908E-16));
#19469=DIRECTION('center_axis',(1.,0.,0.));
#19470=DIRECTION('ref_axis',(0.,1.,0.));
#19471=DIRECTION('center_axis',(-1.,0.,0.));
#19472=DIRECTION('ref_axis',(0.,0.,-1.));
#19473=DIRECTION('center_axis',(-1.,0.,0.));
#19474=DIRECTION('ref_axis',(0.,0.,-1.));
#19475=DIRECTION('',(0.707106781186548,-8.65956056235493E-17,-0.707106781186547));
#19476=DIRECTION('center_axis',(1.,0.,0.));
#19477=DIRECTION('ref_axis',(0.,0.,-1.));
#19478=DIRECTION('center_axis',(1.,0.,0.));
#19479=DIRECTION('ref_axis',(0.,0.,-1.));
#19480=DIRECTION('',(1.,0.,0.));
#19481=DIRECTION('center_axis',(-1.,0.,0.));
#19482=DIRECTION('ref_axis',(0.,0.,-1.));
#19483=DIRECTION('center_axis',(1.,0.,0.));
#19484=DIRECTION('ref_axis',(0.,0.,-1.));
#19485=DIRECTION('center_axis',(-1.,0.,0.));
#19486=DIRECTION('ref_axis',(0.,1.,0.));
#19487=DIRECTION('center_axis',(1.,0.,0.));
#19488=DIRECTION('ref_axis',(0.,0.,-1.));
#19489=DIRECTION('center_axis',(1.,0.,0.));
#19490=DIRECTION('ref_axis',(0.,0.,-1.));
#19491=DIRECTION('',(-0.707106781186548,8.65956056235493E-17,-0.707106781186547));
#19492=DIRECTION('center_axis',(1.,0.,0.));
#19493=DIRECTION('ref_axis',(0.,0.,-1.));
#19494=DIRECTION('center_axis',(0.,0.,1.));
#19495=DIRECTION('ref_axis',(1.,0.,0.));
#19496=DIRECTION('',(-1.,0.,0.));
#19497=DIRECTION('',(1.,0.,0.));
#19498=DIRECTION('center_axis',(0.,-0.5,0.866025403784439));
#19499=DIRECTION('ref_axis',(0.,-0.866025403784439,-0.5));
#19500=DIRECTION('',(-1.,0.,0.));
#19501=DIRECTION('center_axis',(1.,0.,0.));
#19502=DIRECTION('ref_axis',(0.,1.,0.));
#19503=DIRECTION('',(0.506349288588206,-0.862328474507375,-1.05604780611908E-16));
#19504=DIRECTION('center_axis',(0.,-0.866025403784438,0.500000000000002));
#19505=DIRECTION('ref_axis',(1.,0.,0.));
#19506=DIRECTION('',(1.,0.,0.));
#19507=DIRECTION('center_axis',(0.,-1.,-1.37354477598826E-16));
#19508=DIRECTION('ref_axis',(0.,1.37354477598826E-16,-1.));
#19509=DIRECTION('',(-1.,0.,0.));
#19510=DIRECTION('center_axis',(0.,-0.866025403784439,-0.499999999999999));
#19511=DIRECTION('ref_axis',(0.,0.499999999999999,-0.866025403784439));
#19512=DIRECTION('',(1.,0.,0.));
#19513=DIRECTION('center_axis',(0.,0.866025403784438,-0.500000000000002));
#19514=DIRECTION('ref_axis',(-1.,0.,0.));
#19515=DIRECTION('',(-1.,0.,0.));
#19516=DIRECTION('center_axis',(0.,0.5,-0.866025403784439));
#19517=DIRECTION('ref_axis',(0.,0.866025403784439,0.5));
#19518=DIRECTION('',(1.,0.,0.));
#19519=DIRECTION('center_axis',(0.,1.60246890531963E-15,-1.));
#19520=DIRECTION('ref_axis',(-1.,0.,0.));
#19521=DIRECTION('',(-1.,0.,0.));
#19522=DIRECTION('center_axis',(0.,-0.5,-0.866025403784439));
#19523=DIRECTION('ref_axis',(0.,0.866025403784439,-0.5));
#19524=DIRECTION('center_axis',(0.,0.5,0.866025403784439));
#19525=DIRECTION('ref_axis',(0.,-0.866025403784439,0.5));
#19526=DIRECTION('axis',(0.,0.,1.));
#19527=DIRECTION('refdir',(1.,0.,0.));
#19528=DIRECTION('center_axis',(1.,0.,0.));
#19529=DIRECTION('ref_axis',(0.,1.,0.));
#19530=DIRECTION('',(-1.,0.,0.));
#19531=DIRECTION('center_axis',(1.,0.,0.));
#19532=DIRECTION('ref_axis',(0.,1.,0.));
#19533=DIRECTION('center_axis',(1.,0.,0.));
#19534=DIRECTION('ref_axis',(0.,1.,0.));
#19535=DIRECTION('',(-1.,0.,0.));
#19536=DIRECTION('center_axis',(1.,0.,0.));
#19537=DIRECTION('ref_axis',(0.,1.,0.));
#19538=DIRECTION('',(-1.,0.,0.));
#19539=DIRECTION('center_axis',(1.,0.,0.));
#19540=DIRECTION('ref_axis',(0.,1.,0.));
#19541=DIRECTION('',(-1.,0.,0.));
#19542=DIRECTION('center_axis',(1.,0.,0.));
#19543=DIRECTION('ref_axis',(0.,1.,0.));
#19544=DIRECTION('',(-1.,0.,0.));
#19545=DIRECTION('center_axis',(1.,0.,0.));
#19546=DIRECTION('ref_axis',(0.,1.,0.));
#19547=DIRECTION('',(-1.,0.,0.));
#19548=DIRECTION('center_axis',(1.,0.,0.));
#19549=DIRECTION('ref_axis',(0.,1.,0.));
#19550=DIRECTION('',(-1.,0.,0.));
#19551=DIRECTION('center_axis',(1.,0.,0.));
#19552=DIRECTION('ref_axis',(0.,1.,0.));
#19553=DIRECTION('',(-1.,0.,0.));
#19554=DIRECTION('center_axis',(1.,0.,0.));
#19555=DIRECTION('ref_axis',(0.,1.,0.));
#19556=DIRECTION('',(-1.,0.,0.));
#19557=DIRECTION('center_axis',(1.,0.,0.));
#19558=DIRECTION('ref_axis',(0.,1.,0.));
#19559=DIRECTION('',(-1.,0.,0.));
#19560=DIRECTION('center_axis',(1.,0.,0.));
#19561=DIRECTION('ref_axis',(0.,1.,0.));
#19562=DIRECTION('',(-1.,0.,0.));
#19563=DIRECTION('center_axis',(1.,0.,0.));
#19564=DIRECTION('ref_axis',(0.,1.,0.));
#19565=DIRECTION('',(-1.,0.,0.));
#19566=DIRECTION('center_axis',(1.,0.,0.));
#19567=DIRECTION('ref_axis',(0.,1.,0.));
#19568=DIRECTION('',(-1.,0.,0.));
#19569=DIRECTION('center_axis',(1.,0.,0.));
#19570=DIRECTION('ref_axis',(0.,1.,0.));
#19571=DIRECTION('',(-1.,0.,0.));
#19572=DIRECTION('center_axis',(1.,0.,0.));
#19573=DIRECTION('ref_axis',(0.,1.,0.));
#19574=DIRECTION('',(-1.,0.,0.));
#19575=DIRECTION('center_axis',(1.,0.,0.));
#19576=DIRECTION('ref_axis',(0.,1.,0.));
#19577=DIRECTION('',(-1.,0.,0.));
#19578=DIRECTION('center_axis',(1.,0.,0.));
#19579=DIRECTION('ref_axis',(0.,1.,0.));
#19580=DIRECTION('',(-1.,0.,0.));
#19581=DIRECTION('center_axis',(1.,0.,0.));
#19582=DIRECTION('ref_axis',(0.,1.,0.));
#19583=DIRECTION('',(-1.,0.,0.));
#19584=DIRECTION('center_axis',(1.,0.,0.));
#19585=DIRECTION('ref_axis',(0.,1.,0.));
#19586=DIRECTION('center_axis',(1.,0.,0.));
#19587=DIRECTION('ref_axis',(0.,0.449886232649206,-0.893085873627337));
#19588=DIRECTION('',(1.,0.,0.));
#19589=DIRECTION('center_axis',(1.,0.,0.));
#19590=DIRECTION('ref_axis',(0.,1.,1.377013058433E-13));
#19591=DIRECTION('center_axis',(1.,0.,0.));
#19592=DIRECTION('ref_axis',(0.,1.,1.377013058433E-13));
#19593=DIRECTION('',(1.,0.,0.));
#19594=DIRECTION('center_axis',(1.,0.,0.));
#19595=DIRECTION('ref_axis',(0.,1.,1.377013058433E-13));
#19596=DIRECTION('',(1.,0.,0.));
#19597=DIRECTION('center_axis',(1.,0.,0.));
#19598=DIRECTION('ref_axis',(0.,1.,1.377013058433E-13));
#19599=DIRECTION('',(1.,0.,0.));
#19600=DIRECTION('center_axis',(1.,0.,0.));
#19601=DIRECTION('ref_axis',(0.,1.,1.377013058433E-13));
#19602=DIRECTION('',(1.,0.,0.));
#19603=DIRECTION('center_axis',(1.,0.,0.));
#19604=DIRECTION('ref_axis',(0.,1.,1.377013058433E-13));
#19605=DIRECTION('',(1.,0.,0.));
#19606=DIRECTION('center_axis',(1.,0.,0.));
#19607=DIRECTION('ref_axis',(0.,1.,1.377013058433E-13));
#19608=DIRECTION('',(1.,0.,0.));
#19609=DIRECTION('center_axis',(1.,0.,0.));
#19610=DIRECTION('ref_axis',(0.,1.,1.377013058433E-13));
#19611=DIRECTION('',(1.,0.,0.));
#19612=DIRECTION('center_axis',(1.,0.,0.));
#19613=DIRECTION('ref_axis',(0.,1.,1.377013058433E-13));
#19614=DIRECTION('',(1.,0.,0.));
#19615=DIRECTION('center_axis',(1.,0.,0.));
#19616=DIRECTION('ref_axis',(0.,1.,1.377013058433E-13));
#19617=DIRECTION('',(1.,0.,0.));
#19618=DIRECTION('center_axis',(1.,0.,0.));
#19619=DIRECTION('ref_axis',(0.,1.,1.377013058433E-13));
#19620=DIRECTION('',(1.,0.,0.));
#19621=DIRECTION('center_axis',(1.,0.,0.));
#19622=DIRECTION('ref_axis',(0.,1.,1.377013058433E-13));
#19623=DIRECTION('',(1.,0.,0.));
#19624=DIRECTION('center_axis',(1.,0.,0.));
#19625=DIRECTION('ref_axis',(0.,1.,1.377013058433E-13));
#19626=DIRECTION('',(1.,0.,0.));
#19627=DIRECTION('center_axis',(1.,0.,0.));
#19628=DIRECTION('ref_axis',(0.,1.,1.377013058433E-13));
#19629=DIRECTION('',(1.,0.,0.));
#19630=DIRECTION('center_axis',(1.,0.,0.));
#19631=DIRECTION('ref_axis',(0.,1.,1.377013058433E-13));
#19632=DIRECTION('',(1.,0.,0.));
#19633=DIRECTION('center_axis',(1.,0.,0.));
#19634=DIRECTION('ref_axis',(0.,1.,1.377013058433E-13));
#19635=DIRECTION('',(1.,0.,0.));
#19636=DIRECTION('center_axis',(1.,0.,0.));
#19637=DIRECTION('ref_axis',(0.,1.,1.377013058433E-13));
#19638=DIRECTION('',(1.,0.,0.));
#19639=DIRECTION('center_axis',(1.,0.,0.));
#19640=DIRECTION('ref_axis',(0.,0.,-1.));
#19641=DIRECTION('center_axis',(1.,0.,0.));
#19642=DIRECTION('ref_axis',(0.,1.,0.));
#19643=DIRECTION('center_axis',(1.,0.,0.));
#19644=DIRECTION('ref_axis',(0.,1.,0.));
#19645=DIRECTION('center_axis',(-1.,0.,0.));
#19646=DIRECTION('ref_axis',(0.,1.,1.377013058433E-13));
#19647=DIRECTION('center_axis',(1.,0.,0.));
#19648=DIRECTION('ref_axis',(0.,1.,1.377013058433E-13));
#19649=DIRECTION('center_axis',(1.,0.,0.));
#19650=DIRECTION('ref_axis',(0.,1.,0.));
#19651=DIRECTION('',(0.523361335187425,-0.852110857125313,-1.04353483369722E-16));
#19652=DIRECTION('center_axis',(-1.,0.,0.));
#19653=DIRECTION('ref_axis',(0.,1.,0.));
#19654=DIRECTION('center_axis',(0.,-0.5,-0.866025403784439));
#19655=DIRECTION('ref_axis',(0.,-0.866025403784439,0.5));
#19656=DIRECTION('',(-1.,0.,0.));
#19657=DIRECTION('',(0.,-0.866025403784439,0.5));
#19658=DIRECTION('',(-1.,0.,0.));
#19659=DIRECTION('center_axis',(0.,-1.,-1.60246890531964E-16));
#19660=DIRECTION('ref_axis',(0.,-1.60246890531964E-16,1.));
#19661=DIRECTION('',(0.,-1.60246890531964E-16,1.));
#19662=DIRECTION('',(-1.,0.,0.));
#19663=DIRECTION('center_axis',(0.,-0.5,0.866025403784439));
#19664=DIRECTION('ref_axis',(0.,0.866025403784439,0.5));
#19665=DIRECTION('',(0.,0.866025403784439,0.5));
#19666=DIRECTION('',(-1.,0.,0.));
#19667=DIRECTION('center_axis',(0.,0.5,0.866025403784439));
#19668=DIRECTION('ref_axis',(0.,0.866025403784439,-0.5));
#19669=DIRECTION('',(0.,0.866025403784439,-0.5));
#19670=DIRECTION('',(-1.,0.,0.));
#19671=DIRECTION('center_axis',(0.,0.5,-0.866025403784439));
#19672=DIRECTION('ref_axis',(0.,-0.866025403784439,-0.5));
#19673=DIRECTION('',(-1.,0.,0.));
#19674=DIRECTION('',(0.,-0.866025403784439,-0.5));
#19675=DIRECTION('center_axis',(0.,1.,-3.20493781063927E-16));
#19676=DIRECTION('ref_axis',(0.,-3.20493781063927E-16,-1.));
#19677=DIRECTION('',(0.,-3.20493781063927E-16,-1.));
#19678=DIRECTION('center_axis',(-1.,0.,0.));
#19679=DIRECTION('ref_axis',(0.,0.,1.));
#19680=DIRECTION('center_axis',(-1.,0.,0.));
#19681=DIRECTION('ref_axis',(0.,0.,1.));
#19682=DIRECTION('center_axis',(1.,0.,0.));
#19683=DIRECTION('ref_axis',(0.,0.,-1.));
#19684=DIRECTION('center_axis',(1.,0.,0.));
#19685=DIRECTION('ref_axis',(0.,1.,0.));
#19686=DIRECTION('',(-0.707106781186548,0.707106781186547,8.65956056235493E-17));
#19687=DIRECTION('center_axis',(1.,0.,0.));
#19688=DIRECTION('ref_axis',(0.,-0.927547100086637,-0.373706271182154));
#19689=DIRECTION('center_axis',(1.,0.,0.));
#19690=DIRECTION('ref_axis',(0.,1.,0.));
#19691=DIRECTION('center_axis',(-1.,0.,0.));
#19692=DIRECTION('ref_axis',(0.,0.,1.));
#19693=DIRECTION('center_axis',(1.,0.,0.));
#19694=DIRECTION('ref_axis',(0.,0.,-1.));
#19695=DIRECTION('center_axis',(1.,0.,0.));
#19696=DIRECTION('ref_axis',(0.,1.,0.));
#19697=DIRECTION('center_axis',(1.,0.,0.));
#19698=DIRECTION('ref_axis',(0.,0.,-1.));
#19699=DIRECTION('',(-1.,0.,0.));
#19700=DIRECTION('center_axis',(1.,0.,0.));
#19701=DIRECTION('ref_axis',(0.,0.,-1.));
#19702=DIRECTION('',(0.,0.,1.));
#19703=DIRECTION('',(1.,0.,0.));
#19704=DIRECTION('',(0.,0.,1.));
#19705=DIRECTION('',(1.,0.,0.));
#19706=DIRECTION('',(0.,0.,1.));
#19707=DIRECTION('',(1.,0.,0.));
#19708=DIRECTION('',(0.,0.,1.));
#19709=DIRECTION('',(1.,0.,0.));
#19710=DIRECTION('',(0.,0.,1.));
#19711=DIRECTION('',(1.,0.,0.));
#19712=DIRECTION('',(0.,0.,1.));
#19713=DIRECTION('',(1.,0.,0.));
#19714=DIRECTION('',(0.,-6.10622663543836E-16,-1.));
#19715=DIRECTION('',(0.,1.,-6.10622663543836E-16));
#19716=DIRECTION('',(0.,0.,1.));
#19717=DIRECTION('',(1.,0.,0.));
#19718=DIRECTION('',(0.,0.,1.));
#19719=DIRECTION('',(1.,0.,0.));
#19720=DIRECTION('',(0.,6.10622663543836E-16,1.));
#19721=DIRECTION('',(0.999999999999999,0.,0.));
#19722=DIRECTION('',(-1.,0.,0.));
#19723=DIRECTION('',(0.,0.,1.));
#19724=DIRECTION('',(-1.,0.,0.));
#19725=DIRECTION('',(0.,0.,1.));
#19726=DIRECTION('',(1.,0.,0.));
#19727=DIRECTION('',(0.,0.,-1.));
#19728=DIRECTION('',(1.,0.,0.));
#19729=DIRECTION('',(0.,0.,-1.));
#19730=DIRECTION('',(0.,0.,-1.));
#19731=DIRECTION('',(-1.,0.,0.));
#19732=DIRECTION('',(0.,0.,-1.));
#19733=DIRECTION('',(-1.,0.,0.));
#19734=DIRECTION('',(0.,-6.10622663543836E-16,-1.));
#19735=DIRECTION('',(-0.999999999999999,0.,0.));
#19736=DIRECTION('',(-1.,0.,0.));
#19737=DIRECTION('',(0.,0.,1.));
#19738=DIRECTION('',(-1.,0.,0.));
#19739=DIRECTION('',(0.,0.,1.));
#19740=DIRECTION('',(1.,0.,0.));
#19741=DIRECTION('',(0.,0.,-1.));
#19742=DIRECTION('',(1.,0.,0.));
#19743=DIRECTION('',(0.,0.,-1.));
#19744=DIRECTION('',(0.,-6.10622663543836E-16,-1.));
#19745=DIRECTION('',(0.,1.,-6.10622663543836E-16));
#19746=DIRECTION('',(0.,-6.10622663543836E-16,-1.));
#19747=DIRECTION('',(0.,1.,-6.10622663543836E-16));
#19748=CARTESIAN_POINT('',(0.,0.,0.));
#19749=CARTESIAN_POINT('',(0.,0.,0.));
#19750=CARTESIAN_POINT('Origin',(20.2248703552884,-6.,0.7398357130565));
#19751=CARTESIAN_POINT('',(20.2359894539709,5.74912062451897,0.729120624518965));
#19752=CARTESIAN_POINT('',(20.4737490231322,5.52,0.5));
#19753=CARTESIAN_POINT('',(16.044254314835,9.78854993659521,4.7685499365952));
#19754=CARTESIAN_POINT('',(20.4737490231322,-5.52,0.5));
#19755=CARTESIAN_POINT('',(20.4737490231322,-6.,0.5));
#19756=CARTESIAN_POINT('',(20.2359894539709,-5.74912062451896,0.72912062451896));
#19757=CARTESIAN_POINT('',(14.0206695716018,-11.7386081478045,6.71860814780449));
#19758=CARTESIAN_POINT('',(19.9759916874447,-5.5,0.979671426113));
#19759=CARTESIAN_POINT('Ctrl Pts',(20.2359894539709,-5.74912062451896,0.72912062451896));
#19760=CARTESIAN_POINT('Ctrl Pts',(20.1051859468429,-5.62294071733703,0.855171413339531));
#19761=CARTESIAN_POINT('Ctrl Pts',(19.9759916874447,-5.5,0.979671426112999));
#19762=CARTESIAN_POINT('',(19.9759916874447,5.5,0.979671426113));
#19763=CARTESIAN_POINT('',(19.9759916874447,-6.,0.979671426113));
#19764=CARTESIAN_POINT('Ctrl Pts',(19.9759916874446,5.5,0.979671426113002));
#19765=CARTESIAN_POINT('Ctrl Pts',(20.1051859468428,5.6229407173369,0.855171413339668));
#19766=CARTESIAN_POINT('Ctrl Pts',(20.2359894539709,5.74912062451897,0.729120624518965));
#19767=CARTESIAN_POINT('Origin',(-14.9979165219706,5.76,0.74));
#19768=CARTESIAN_POINT('',(20.4765622114651,6.,0.98));
#19769=CARTESIAN_POINT('Ctrl Pts',(20.2359894539709,5.74912062451897,0.729120624518965));
#19770=CARTESIAN_POINT('Ctrl Pts',(20.3562758327179,5.87381908208973,0.853819082089724));
#19771=CARTESIAN_POINT('Ctrl Pts',(20.4765622114651,6.,0.98));
#19772=CARTESIAN_POINT('',(45.17,6.,0.98));
#19773=CARTESIAN_POINT('',(-14.9979165219706,6.,0.98));
#19774=CARTESIAN_POINT('',(45.17,5.52,0.5));
#19775=CARTESIAN_POINT('',(45.17,6.,0.98));
#19776=CARTESIAN_POINT('',(-14.9979165219706,5.52,0.5));
#19777=CARTESIAN_POINT('Origin',(0.,5.75,0.));
#19778=CARTESIAN_POINT('',(-19.9759916874447,5.5,0.979671426113));
#19779=CARTESIAN_POINT('Origin',(0.,5.5,0.));
#19780=CARTESIAN_POINT('',(-20.2359894539709,5.74912062451897,0.729120624518964));
#19781=CARTESIAN_POINT('Ctrl Pts',(-20.2359894539709,5.74912062451897,0.729120624518964));
#19782=CARTESIAN_POINT('Ctrl Pts',(-20.105185946843,5.62294071733708,0.855171413339494));
#19783=CARTESIAN_POINT('Ctrl Pts',(-19.9759916874447,5.5,0.979671426113));
#19784=CARTESIAN_POINT('',(-20.4765622114651,6.,0.98));
#19785=CARTESIAN_POINT('Ctrl Pts',(-20.4765622114651,6.,0.98));
#19786=CARTESIAN_POINT('Ctrl Pts',(-20.356275832718,5.87381908208979,0.853819082089789));
#19787=CARTESIAN_POINT('Ctrl Pts',(-20.2359894539709,5.74912062451897,0.729120624518963));
#19788=CARTESIAN_POINT('Origin',(0.,6.,0.));
#19789=CARTESIAN_POINT('Origin',(0.,-6.,0.));
#19790=CARTESIAN_POINT('',(-19.9759916874447,-5.5,0.979671426113));
#19791=CARTESIAN_POINT('Origin',(0.,-5.5,0.));
#19792=CARTESIAN_POINT('',(-19.9759916874447,-6.,0.979671426113));
#19793=CARTESIAN_POINT('Origin',(45.17,5.52,0.5));
#19794=CARTESIAN_POINT('',(45.65,5.52,0.98));
#19795=CARTESIAN_POINT('',(45.65,5.52,0.98));
#19796=CARTESIAN_POINT('',(45.17,5.52,0.5));
#19797=CARTESIAN_POINT('Origin',(45.17,-6.,0.98));
#19798=CARTESIAN_POINT('',(45.65,-5.52,0.98));
#19799=CARTESIAN_POINT('',(45.17,-5.52,0.5));
#19800=CARTESIAN_POINT('',(45.65,-5.52,0.98));
#19801=CARTESIAN_POINT('',(45.17,-6.,0.98));
#19802=CARTESIAN_POINT('',(45.17,-6.,0.98));
#19803=CARTESIAN_POINT('',(45.17,-5.52,0.5));
#19804=CARTESIAN_POINT('Origin',(45.41,-5.76,3.));
#19805=CARTESIAN_POINT('',(45.65,-5.52,4.));
#19806=CARTESIAN_POINT('',(45.17,-6.,4.));
#19807=CARTESIAN_POINT('',(45.65,-5.52,4.));
#19808=CARTESIAN_POINT('',(45.17,-6.,3.));
#19809=CARTESIAN_POINT('',(45.65,-5.52,3.));
#19810=CARTESIAN_POINT('Origin',(43.65,-5.76,4.));
#19811=CARTESIAN_POINT('',(43.65,-5.52,6.));
#19812=CARTESIAN_POINT('Origin',(43.65,-5.52,4.));
#19813=CARTESIAN_POINT('',(43.65,-6.,5.52));
#19814=CARTESIAN_POINT('',(43.65,-5.52,6.));
#19815=CARTESIAN_POINT('Origin',(43.65,-6.,4.));
#19816=CARTESIAN_POINT('Origin',(14.6969384566991,-5.76,5.76));
#19817=CARTESIAN_POINT('',(29.3734642151722,-5.52,6.));
#19818=CARTESIAN_POINT('',(28.9789509817039,-6.,5.52));
#19819=CARTESIAN_POINT('Ctrl Pts',(28.9789509817039,-6.,5.52));
#19820=CARTESIAN_POINT('Ctrl Pts',(29.1762075984394,-5.76162260937474,5.75837739062526));
#19821=CARTESIAN_POINT('Ctrl Pts',(29.3734642151722,-5.52,6.));
#19822=CARTESIAN_POINT('',(14.6969384566991,-6.,5.52));
#19823=CARTESIAN_POINT('',(14.6969384566991,-5.52,6.));
#19824=CARTESIAN_POINT('Origin',(-14.9979165219706,-5.76,0.74));
#19825=CARTESIAN_POINT('',(-14.9979165219706,-5.52,0.5));
#19826=CARTESIAN_POINT('',(20.4765622114651,-6.,0.98));
#19827=CARTESIAN_POINT('',(-14.9979165219706,-6.,0.98));
#19828=CARTESIAN_POINT('Ctrl Pts',(20.4765622114651,-6.,0.98));
#19829=CARTESIAN_POINT('Ctrl Pts',(20.356275832718,-5.87381908208979,0.853819082089787));
#19830=CARTESIAN_POINT('Ctrl Pts',(20.2359894539709,-5.74912062451896,0.729120624518961));
#19831=CARTESIAN_POINT('Origin',(45.41,-6.,0.74));
#19832=CARTESIAN_POINT('',(45.65,-6.,0.98));
#19833=CARTESIAN_POINT('',(45.17,-6.,0.5));
#19834=CARTESIAN_POINT('Origin',(14.6969384566991,5.76,5.76));
#19835=CARTESIAN_POINT('',(28.9789509817039,6.,5.52));
#19836=CARTESIAN_POINT('',(29.3734642151722,5.52,6.));
#19837=CARTESIAN_POINT('Ctrl Pts',(29.3734642151722,5.52,6.));
#19838=CARTESIAN_POINT('Ctrl Pts',(29.1762075984394,5.76162260937474,5.75837739062526));
#19839=CARTESIAN_POINT('Ctrl Pts',(28.9789509817039,6.,5.52));
#19840=CARTESIAN_POINT('',(43.65,5.52,6.));
#19841=CARTESIAN_POINT('',(14.6969384566991,5.52,6.));
#19842=CARTESIAN_POINT('',(43.65,6.,5.52));
#19843=CARTESIAN_POINT('',(43.65,5.52,6.));
#19844=CARTESIAN_POINT('',(14.6969384566991,6.,5.52));
#19845=CARTESIAN_POINT('Origin',(43.65,5.76,4.));
#19846=CARTESIAN_POINT('',(45.65,5.52,4.));
#19847=CARTESIAN_POINT('Origin',(43.65,5.52,4.));
#19848=CARTESIAN_POINT('',(45.17,6.,4.));
#19849=CARTESIAN_POINT('',(45.65,5.52,4.));
#19850=CARTESIAN_POINT('Origin',(43.65,6.,4.));
#19851=CARTESIAN_POINT('Origin',(45.41,5.76,3.));
#19852=CARTESIAN_POINT('',(45.65,5.52,3.));
#19853=CARTESIAN_POINT('',(45.17,6.,3.));
#19854=CARTESIAN_POINT('Origin',(0.,-6.,0.));
#19855=CARTESIAN_POINT('',(-28.9789509817039,-6.,5.52));
#19856=CARTESIAN_POINT('Origin',(0.,-6.,0.));
#19857=CARTESIAN_POINT('',(-43.65,-6.,5.52));
#19858=CARTESIAN_POINT('',(-22.825,-6.,5.52));
#19859=CARTESIAN_POINT('',(-45.17,-6.,4.));
#19860=CARTESIAN_POINT('Origin',(-43.65,-6.,4.));
#19861=CARTESIAN_POINT('',(-45.17,-6.,0.98));
#19862=CARTESIAN_POINT('',(-45.17,-6.,0.25));
#19863=CARTESIAN_POINT('',(-20.4765622114651,-6.,0.98));
#19864=CARTESIAN_POINT('',(-14.9979165219706,-6.,0.98));
#19865=CARTESIAN_POINT('Origin',(0.,-6.,0.));
#19866=CARTESIAN_POINT('Origin',(45.65,-6.,6.));
#19867=CARTESIAN_POINT('',(45.65,-6.,4.));
#19868=CARTESIAN_POINT('Origin',(43.65,-6.,4.));
#19869=CARTESIAN_POINT('',(43.65,-6.,6.));
#19870=CARTESIAN_POINT('Origin',(29.3938769133981,-6.,6.));
#19871=CARTESIAN_POINT('',(29.3938769133981,5.5,6.));
#19872=CARTESIAN_POINT('Ctrl Pts',(29.3734642151722,5.51999999999998,6.));
#19873=CARTESIAN_POINT('Ctrl Pts',(29.3836671610351,5.51000347347589,6.));
#19874=CARTESIAN_POINT('Ctrl Pts',(29.3938769133981,5.5,6.));
#19875=CARTESIAN_POINT('',(29.3938769133981,-5.5,6.));
#19876=CARTESIAN_POINT('',(29.3938769133981,-6.,6.));
#19877=CARTESIAN_POINT('Ctrl Pts',(29.3938769133981,-5.5,6.));
#19878=CARTESIAN_POINT('Ctrl Pts',(29.3836671610351,-5.51000347347589,6.));
#19879=CARTESIAN_POINT('Ctrl Pts',(29.3734642151722,-5.51999999999997,6.));
#19880=CARTESIAN_POINT('',(37.25,-2.75545529808154E-16,6.));
#19881=CARTESIAN_POINT('Origin',(39.5,0.,6.));
#19882=CARTESIAN_POINT('Origin',(-20.2248703552884,-6.,0.7398357130565));
#19883=CARTESIAN_POINT('',(-20.2359894539709,-5.74912062451896,0.729120624518962));
#19884=CARTESIAN_POINT('',(-20.4737490231322,-5.52,0.5));
#19885=CARTESIAN_POINT('',(-19.2696493386723,-6.68034897211366,1.66034897211366));
#19886=CARTESIAN_POINT('',(-20.4737490231322,5.52,0.5));
#19887=CARTESIAN_POINT('',(-20.4737490231322,-6.,0.5));
#19888=CARTESIAN_POINT('',(-21.2932340819055,4.73029076090437,-0.289709239095627));
#19889=CARTESIAN_POINT('Ctrl Pts',(-19.9759916874447,-5.5,0.979671426112999));
#19890=CARTESIAN_POINT('Ctrl Pts',(-20.1051859468429,-5.62294071733703,
0.855171413339532));
#19891=CARTESIAN_POINT('Ctrl Pts',(-20.2359894539709,-5.74912062451896,
0.729120624518962));
#19892=CARTESIAN_POINT('Origin',(-14.9979165219706,5.76,0.74));
#19893=CARTESIAN_POINT('',(-45.17,5.52,0.5));
#19894=CARTESIAN_POINT('',(-14.9979165219706,5.52,0.5));
#19895=CARTESIAN_POINT('',(-45.17,6.,0.98));
#19896=CARTESIAN_POINT('',(-45.17,5.52,0.5));
#19897=CARTESIAN_POINT('',(-14.9979165219706,6.,0.98));
#19898=CARTESIAN_POINT('Origin',(-45.65,5.52,0.98));
#19899=CARTESIAN_POINT('',(-45.65,5.52,0.98));
#19900=CARTESIAN_POINT('',(-45.65,5.52,0.98));
#19901=CARTESIAN_POINT('',(-45.17,6.,0.98));
#19902=CARTESIAN_POINT('Origin',(-45.17,-6.,0.98));
#19903=CARTESIAN_POINT('',(-45.17,-5.52,0.5));
#19904=CARTESIAN_POINT('',(-45.65,-5.52,0.98));
#19905=CARTESIAN_POINT('',(-45.17,-5.52,0.5));
#19906=CARTESIAN_POINT('',(-45.17,-6.,0.98));
#19907=CARTESIAN_POINT('',(-45.65,-5.52,0.98));
#19908=CARTESIAN_POINT('Origin',(-14.9979165219706,-5.76,0.74));
#19909=CARTESIAN_POINT('Ctrl Pts',(-20.2359894539709,-5.74912062451896,
0.729120624518962));
#19910=CARTESIAN_POINT('Ctrl Pts',(-20.3562758327179,-5.87381908208974,
0.853819082089735));
#19911=CARTESIAN_POINT('Ctrl Pts',(-20.4765622114651,-6.,0.98));
#19912=CARTESIAN_POINT('',(-14.9979165219706,-5.52,0.5));
#19913=CARTESIAN_POINT('Origin',(-22.825,-5.76,5.76));
#19914=CARTESIAN_POINT('',(-29.3734642151722,-5.52,6.));
#19915=CARTESIAN_POINT('Ctrl Pts',(-29.3734642151722,-5.52,6.));
#19916=CARTESIAN_POINT('Ctrl Pts',(-29.1762075984394,-5.76162260937474,
5.75837739062526));
#19917=CARTESIAN_POINT('Ctrl Pts',(-28.9789509817039,-6.,5.52));
#19918=CARTESIAN_POINT('',(-43.65,-5.52,6.));
#19919=CARTESIAN_POINT('',(-22.825,-5.52,6.));
#19920=CARTESIAN_POINT('',(-43.65,-5.52,6.));
#19921=CARTESIAN_POINT('Origin',(-43.65,-5.76,4.));
#19922=CARTESIAN_POINT('',(-45.65,-5.52,4.));
#19923=CARTESIAN_POINT('Origin',(-43.65,-5.52,4.));
#19924=CARTESIAN_POINT('',(-45.65,-5.52,4.));
#19925=CARTESIAN_POINT('Origin',(-45.41,-5.76,0.25));
#19926=CARTESIAN_POINT('',(-45.65,-5.52,0.25));
#19927=CARTESIAN_POINT('Origin',(-45.41,-6.,0.74));
#19928=CARTESIAN_POINT('',(-45.17,-6.,0.5));
#19929=CARTESIAN_POINT('',(-45.65,-6.,0.98));
#19930=CARTESIAN_POINT('Origin',(-45.41,5.76,0.25));
#19931=CARTESIAN_POINT('',(-45.65,5.52,4.));
#19932=CARTESIAN_POINT('',(-45.17,6.,4.));
#19933=CARTESIAN_POINT('',(-45.65,5.52,4.));
#19934=CARTESIAN_POINT('',(-45.17,6.,0.25));
#19935=CARTESIAN_POINT('',(-45.65,5.52,0.25));
#19936=CARTESIAN_POINT('Origin',(-43.65,5.76,4.));
#19937=CARTESIAN_POINT('',(-43.65,5.52,6.));
#19938=CARTESIAN_POINT('Origin',(-43.65,5.52,4.));
#19939=CARTESIAN_POINT('',(-43.65,6.,5.52));
#19940=CARTESIAN_POINT('',(-43.65,5.52,6.));
#19941=CARTESIAN_POINT('Origin',(-43.65,6.,4.));
#19942=CARTESIAN_POINT('Origin',(-22.825,5.76,5.76));
#19943=CARTESIAN_POINT('',(-29.3734642151722,5.52,6.));
#19944=CARTESIAN_POINT('',(-28.9789509817039,6.,5.52));
#19945=CARTESIAN_POINT('Ctrl Pts',(-28.9789509817039,6.,5.52));
#19946=CARTESIAN_POINT('Ctrl Pts',(-29.1762075984394,5.76162260937474,5.75837739062526));
#19947=CARTESIAN_POINT('Ctrl Pts',(-29.3734642151722,5.52,6.));
#19948=CARTESIAN_POINT('',(-22.825,6.,5.52));
#19949=CARTESIAN_POINT('',(-22.825,5.52,6.));
#19950=CARTESIAN_POINT('Origin',(0.,-5.75,0.));
#19951=CARTESIAN_POINT('Origin',(-29.9958330439413,-6.,0.5));
#19952=CARTESIAN_POINT('',(-41.75,-2.75545529808155E-16,0.5));
#19953=CARTESIAN_POINT('Origin',(-39.5,0.,0.5));
#19954=CARTESIAN_POINT('Origin',(0.,-5.75,0.));
#19955=CARTESIAN_POINT('',(-29.3938769133981,-5.5,6.));
#19956=CARTESIAN_POINT('Ctrl Pts',(-29.3734642151722,-5.51999999999998,
6.));
#19957=CARTESIAN_POINT('Ctrl Pts',(-29.3836671610351,-5.51000347347589,
6.));
#19958=CARTESIAN_POINT('Ctrl Pts',(-29.3938769133981,-5.5,6.));
#19959=CARTESIAN_POINT('Origin',(0.,-5.5,0.));
#19960=CARTESIAN_POINT('Origin',(0.,5.75,0.));
#19961=CARTESIAN_POINT('',(-29.3938769133981,5.5,6.));
#19962=CARTESIAN_POINT('Ctrl Pts',(-29.3938769133981,5.5,6.));
#19963=CARTESIAN_POINT('Ctrl Pts',(-29.3836671610351,5.51000347347589,6.));
#19964=CARTESIAN_POINT('Ctrl Pts',(-29.3734642151722,5.51999999999998,6.));
#19965=CARTESIAN_POINT('Origin',(0.,5.5,0.));
#19966=CARTESIAN_POINT('Origin',(0.,6.,0.));
#19967=CARTESIAN_POINT('Origin',(0.,-6.,0.));
#19968=CARTESIAN_POINT('',(-29.3938769133981,-6.,6.));
#19969=CARTESIAN_POINT('Origin',(39.5,0.,6.));
#19970=CARTESIAN_POINT('',(37.25,-2.75545529808154E-16,0.5));
#19971=CARTESIAN_POINT('',(37.25,2.75545529808154E-16,6.));
#19972=CARTESIAN_POINT('Origin',(39.5,0.,0.5));
#19973=CARTESIAN_POINT('Origin',(-39.5,0.,6.));
#19974=CARTESIAN_POINT('',(-41.75,-2.75545529808155E-16,6.));
#19975=CARTESIAN_POINT('Origin',(-39.5,0.,6.));
#19976=CARTESIAN_POINT('',(-41.75,2.75545529808155E-16,6.));
#19977=CARTESIAN_POINT('Origin',(0.,6.,0.));
#19978=CARTESIAN_POINT('Origin',(-43.65,-6.,4.));
#19979=CARTESIAN_POINT('',(-43.65,-6.,6.));
#19980=CARTESIAN_POINT('',(-45.65,-6.,4.));
#19981=CARTESIAN_POINT('Origin',(-45.65,-6.,6.));
#19982=CARTESIAN_POINT('Origin',(-45.65,-6.,0.5));
#19983=CARTESIAN_POINT('Origin',(-29.9958330439413,-6.,0.5));
#19984=CARTESIAN_POINT('',(0.,0.,0.));
#19985=CARTESIAN_POINT('Origin',(-30.64,-5.76,-12.225));
#19986=CARTESIAN_POINT('',(-30.4,-5.52,-20.2));
#19987=CARTESIAN_POINT('',(-30.88,-6.,-19.72));
#19988=CARTESIAN_POINT('',(-28.6708476104047,-3.79084761040473,-21.9291523895953));
#19989=CARTESIAN_POINT('',(-30.88,-6.,-34.5));
#19990=CARTESIAN_POINT('',(-30.88,-6.,-12.225));
#19991=CARTESIAN_POINT('',(-30.4,-5.52,-34.5));
#19992=CARTESIAN_POINT('',(-30.88,-6.,-34.5));
#19993=CARTESIAN_POINT('',(-30.4,-5.52,-12.225));
#19994=CARTESIAN_POINT('Origin',(-30.64,-2.,-34.5));
#19995=CARTESIAN_POINT('',(-30.88,-2.,-38.5));
#19996=CARTESIAN_POINT('Origin',(-30.88,-2.,-34.5));
#19997=CARTESIAN_POINT('',(-30.4,-2.,-38.02));
#19998=CARTESIAN_POINT('',(-30.88,-2.,-38.5));
#19999=CARTESIAN_POINT('Origin',(-30.4,-2.,-34.5));
#20000=CARTESIAN_POINT('Origin',(-30.64,-6.,-38.26));
#20001=CARTESIAN_POINT('',(-30.88,2.,-38.5));
#20002=CARTESIAN_POINT('',(-30.4,2.,-38.02));
#20003=CARTESIAN_POINT('',(-30.88,2.,-38.5));
#20004=CARTESIAN_POINT('',(-30.4,-6.,-38.02));
#20005=CARTESIAN_POINT('',(-30.88,-6.,-38.5));
#20006=CARTESIAN_POINT('Origin',(-30.64,2.,-34.5));
#20007=CARTESIAN_POINT('',(-30.88,6.,-34.5));
#20008=CARTESIAN_POINT('Origin',(-30.88,2.,-34.5));
#20009=CARTESIAN_POINT('',(-30.4,5.52,-34.5));
#20010=CARTESIAN_POINT('',(-30.88,6.,-34.5));
#20011=CARTESIAN_POINT('Origin',(-30.4,2.,-34.5));
#20012=CARTESIAN_POINT('Origin',(-30.64,5.76,-12.225));
#20013=CARTESIAN_POINT('',(-30.4,5.52,-20.2));
#20014=CARTESIAN_POINT('',(-30.4,5.52,-12.225));
#20015=CARTESIAN_POINT('',(-30.88,6.,-19.72));
#20016=CARTESIAN_POINT('',(-30.88,6.,-12.225));
#20017=CARTESIAN_POINT('',(-30.88,6.,-19.72));
#20018=CARTESIAN_POINT('Origin',(-11.0900856624284,5.76,-19.96));
#20019=CARTESIAN_POINT('',(-21.9401823146482,6.,-19.72));
#20020=CARTESIAN_POINT('',(-11.0900856624284,6.,-19.72));
#20021=CARTESIAN_POINT('',(-22.1531126481134,5.52,-20.2));
#20022=CARTESIAN_POINT('Ctrl Pts',(-22.1531126481134,5.52,-20.2));
#20023=CARTESIAN_POINT('Ctrl Pts',(-22.0466474813905,5.76115898072722,-19.9588410192728));
#20024=CARTESIAN_POINT('Ctrl Pts',(-21.9401823146482,6.,-19.72));
#20025=CARTESIAN_POINT('',(-11.0900856624284,5.52,-20.2));
#20026=CARTESIAN_POINT('Origin',(-30.4,-6.,-20.2));
#20027=CARTESIAN_POINT('',(-30.4,-6.,-20.2));
#20028=CARTESIAN_POINT('',(-30.4,2.63299061816681E-16,-30.85));
#20029=CARTESIAN_POINT('Origin',(-30.4,0.,-33.));
#20030=CARTESIAN_POINT('Origin',(-22.1801713248568,-6.,-20.2));
#20031=CARTESIAN_POINT('',(-22.1801713248568,5.5,-20.2));
#20032=CARTESIAN_POINT('Ctrl Pts',(-22.1531126481135,5.51999999999993,-20.2));
#20033=CARTESIAN_POINT('Ctrl Pts',(-22.1666374752019,5.51000610346768,-20.2));
#20034=CARTESIAN_POINT('Ctrl Pts',(-22.1801713248568,5.5,-20.2));
#20035=CARTESIAN_POINT('',(-22.1801713248568,-5.5,-20.2));
#20036=CARTESIAN_POINT('',(-22.1801713248568,-6.,-20.2));
#20037=CARTESIAN_POINT('',(-22.1531126481134,-5.52,-20.2));
#20038=CARTESIAN_POINT('Ctrl Pts',(-22.1801713248568,-5.5,-20.2));
#20039=CARTESIAN_POINT('Ctrl Pts',(-22.1666374752019,-5.51000610346768,
-20.2));
#20040=CARTESIAN_POINT('Ctrl Pts',(-22.1531126481134,-5.51999999999993,
-20.2));
#20041=CARTESIAN_POINT('',(-11.0900856624284,-5.52,-20.2));
#20042=CARTESIAN_POINT('Origin',(-17.2,5.76,-5.76));
#20043=CARTESIAN_POINT('',(-34.4,5.52,-6.));
#20044=CARTESIAN_POINT('',(-43.65,5.52,-6.));
#20045=CARTESIAN_POINT('',(-17.2,5.52,-6.));
#20046=CARTESIAN_POINT('',(-43.65,6.,-5.52));
#20047=CARTESIAN_POINT('',(-43.65,5.52,-6.));
#20048=CARTESIAN_POINT('',(-33.92,6.,-5.52));
#20049=CARTESIAN_POINT('',(-17.2,6.,-5.52));
#20050=CARTESIAN_POINT('',(-33.92,6.,-5.52));
#20051=CARTESIAN_POINT('Origin',(-34.16,-5.76,-21.375));
#20052=CARTESIAN_POINT('',(-34.4,-5.52,-6.));
#20053=CARTESIAN_POINT('',(-34.4,-5.52,-34.5));
#20054=CARTESIAN_POINT('',(-34.4,-5.52,-21.375));
#20055=CARTESIAN_POINT('',(-33.92,-6.,-34.5));
#20056=CARTESIAN_POINT('',(-34.4,-5.52,-34.5));
#20057=CARTESIAN_POINT('',(-33.92,-6.,-5.52));
#20058=CARTESIAN_POINT('',(-33.92,-6.,-21.375));
#20059=CARTESIAN_POINT('',(-33.92,-6.,-5.52));
#20060=CARTESIAN_POINT('Origin',(-17.2,-5.76,-5.76));
#20061=CARTESIAN_POINT('',(-43.65,-6.,-5.52));
#20062=CARTESIAN_POINT('',(-17.2,-6.,-5.52));
#20063=CARTESIAN_POINT('',(-43.65,-5.52,-6.));
#20064=CARTESIAN_POINT('',(-43.65,-6.,-5.52));
#20065=CARTESIAN_POINT('',(-17.2,-5.52,-6.));
#20066=CARTESIAN_POINT('Origin',(-43.65,-5.76,-4.));
#20067=CARTESIAN_POINT('',(-45.17,-6.,-4.));
#20068=CARTESIAN_POINT('',(-45.65,-5.52,-4.));
#20069=CARTESIAN_POINT('',(-45.17,-6.,-4.));
#20070=CARTESIAN_POINT('Origin',(-43.65,-5.52,-4.));
#20071=CARTESIAN_POINT('Origin',(-43.65,-6.,-4.));
#20072=CARTESIAN_POINT('Origin',(-45.41,-5.76,-5.125));
#20073=CARTESIAN_POINT('',(-45.41,-5.76,-0.74));
#20074=CARTESIAN_POINT('',(-45.65,-5.52,-0.98));
#20075=CARTESIAN_POINT('',(-46.1008333333333,-5.06916666666667,-1.43083333333333));
#20076=CARTESIAN_POINT('',(-45.65,-5.52,-5.125));
#20077=CARTESIAN_POINT('',(-45.17,-6.,-0.98));
#20078=CARTESIAN_POINT('',(-45.17,-6.,-5.125));
#20079=CARTESIAN_POINT('',(-34.6111805796715,-16.5588194203284,-11.5388194203284));
#20080=CARTESIAN_POINT('Origin',(-34.16,-2.,-34.5));
#20081=CARTESIAN_POINT('',(-34.4,-2.,-38.02));
#20082=CARTESIAN_POINT('',(-33.92,-2.,-38.5));
#20083=CARTESIAN_POINT('',(-34.4,-2.,-38.02));
#20084=CARTESIAN_POINT('Origin',(-33.92,-2.,-34.5));
#20085=CARTESIAN_POINT('Origin',(-34.4,-2.,-34.5));
#20086=CARTESIAN_POINT('Origin',(-34.16,-6.,-38.26));
#20087=CARTESIAN_POINT('',(-34.4,2.,-38.02));
#20088=CARTESIAN_POINT('',(-33.92,2.,-38.5));
#20089=CARTESIAN_POINT('',(-34.4,2.,-38.02));
#20090=CARTESIAN_POINT('',(-33.92,-6.,-38.5));
#20091=CARTESIAN_POINT('',(-34.4,-6.,-38.02));
#20092=CARTESIAN_POINT('Origin',(-34.16,2.,-34.5));
#20093=CARTESIAN_POINT('',(-34.4,5.52,-34.5));
#20094=CARTESIAN_POINT('',(-33.92,6.,-34.5));
#20095=CARTESIAN_POINT('',(-34.4,5.52,-34.5));
#20096=CARTESIAN_POINT('Origin',(-33.92,2.,-34.5));
#20097=CARTESIAN_POINT('Origin',(-34.4,2.,-34.5));
#20098=CARTESIAN_POINT('Origin',(-34.16,5.76,-21.375));
#20099=CARTESIAN_POINT('',(-33.92,6.,-21.375));
#20100=CARTESIAN_POINT('',(-34.4,5.52,-21.375));
#20101=CARTESIAN_POINT('Origin',(-43.65,5.76,-4.));
#20102=CARTESIAN_POINT('',(-45.65,5.52,-4.));
#20103=CARTESIAN_POINT('Origin',(-43.65,5.52,-4.));
#20104=CARTESIAN_POINT('',(-45.17,6.,-4.));
#20105=CARTESIAN_POINT('',(-45.65,5.52,-4.));
#20106=CARTESIAN_POINT('Origin',(-43.65,6.,-4.));
#20107=CARTESIAN_POINT('Origin',(-45.41,5.76,-5.125));
#20108=CARTESIAN_POINT('',(-45.41,5.76,-0.74));
#20109=CARTESIAN_POINT('',(-45.17,6.,-0.98));
#20110=CARTESIAN_POINT('',(-34.6111805796715,16.5588194203284,-11.5388194203284));
#20111=CARTESIAN_POINT('',(-45.17,6.,-5.125));
#20112=CARTESIAN_POINT('',(-45.65,5.52,-0.98));
#20113=CARTESIAN_POINT('',(-45.65,5.52,-5.125));
#20114=CARTESIAN_POINT('',(-48.1008333333333,3.06916666666667,-3.43083333333333));
#20115=CARTESIAN_POINT('Origin',(0.,-6.,-4.25));
#20116=CARTESIAN_POINT('',(-21.9401823146482,-6.,-19.72));
#20117=CARTESIAN_POINT('',(-11.0900856624284,-6.,-19.72));
#20118=CARTESIAN_POINT('',(21.9401823146482,-6.,-19.72));
#20119=CARTESIAN_POINT('Origin',(0.,-6.,0.));
#20120=CARTESIAN_POINT('',(30.88,-6.,-19.72));
#20121=CARTESIAN_POINT('',(15.2,-6.,-19.72));
#20122=CARTESIAN_POINT('',(30.88,-6.,-34.5));
#20123=CARTESIAN_POINT('',(30.88,-6.,-21.375));
#20124=CARTESIAN_POINT('',(33.92,-6.,-34.5));
#20125=CARTESIAN_POINT('',(17.2,-6.,-34.5));
#20126=CARTESIAN_POINT('',(33.92,-6.,-5.52));
#20127=CARTESIAN_POINT('',(33.92,-6.,-5.125));
#20128=CARTESIAN_POINT('',(43.65,-6.,-5.52));
#20129=CARTESIAN_POINT('',(22.825,-6.,-5.52));
#20130=CARTESIAN_POINT('',(45.17,-6.,-4.));
#20131=CARTESIAN_POINT('Origin',(43.65,-6.,-4.));
#20132=CARTESIAN_POINT('',(45.17,-6.,-0.98));
#20133=CARTESIAN_POINT('',(45.17,-6.,-2.375));
#20134=CARTESIAN_POINT('',(20.4765622114651,-6.,-0.98));
#20135=CARTESIAN_POINT('',(14.9979165219706,-6.,-0.98));
#20136=CARTESIAN_POINT('',(-20.4765622114651,-6.,-0.98));
#20137=CARTESIAN_POINT('Origin',(0.,-6.,0.));
#20138=CARTESIAN_POINT('',(14.9979165219706,-6.,-0.98));
#20139=CARTESIAN_POINT('',(-15.2,-6.,-34.5));
#20140=CARTESIAN_POINT('Origin',(-15.2,-2.,-34.5));
#20141=CARTESIAN_POINT('',(-15.2,-2.,-38.5));
#20142=CARTESIAN_POINT('Origin',(-30.4,-6.,-38.5));
#20143=CARTESIAN_POINT('',(-15.2,2.,-38.5));
#20144=CARTESIAN_POINT('Origin',(-15.2,2.,-34.5));
#20145=CARTESIAN_POINT('',(-15.2,6.,-34.5));
#20146=CARTESIAN_POINT('Origin',(0.,6.,-4.25));
#20147=CARTESIAN_POINT('',(-20.4765622114651,6.,-0.98));
#20148=CARTESIAN_POINT('',(14.9979165219706,6.,-0.98));
#20149=CARTESIAN_POINT('',(20.4765622114651,6.,-0.98));
#20150=CARTESIAN_POINT('Origin',(0.,6.,0.));
#20151=CARTESIAN_POINT('',(45.17,6.,-0.98));
#20152=CARTESIAN_POINT('',(14.9979165219706,6.,-0.98));
#20153=CARTESIAN_POINT('',(45.17,6.,-4.));
#20154=CARTESIAN_POINT('',(45.17,6.,-2.375));
#20155=CARTESIAN_POINT('',(43.65,6.,-5.52));
#20156=CARTESIAN_POINT('Origin',(43.65,6.,-4.));
#20157=CARTESIAN_POINT('',(33.92,6.,-5.52));
#20158=CARTESIAN_POINT('',(22.825,6.,-5.52));
#20159=CARTESIAN_POINT('',(33.92,6.,-34.5));
#20160=CARTESIAN_POINT('',(33.92,6.,-5.125));
#20161=CARTESIAN_POINT('',(30.88,6.,-34.5));
#20162=CARTESIAN_POINT('',(17.2,6.,-34.5));
#20163=CARTESIAN_POINT('',(30.88,6.,-19.72));
#20164=CARTESIAN_POINT('',(30.88,6.,-21.375));
#20165=CARTESIAN_POINT('',(21.9401823146482,6.,-19.72));
#20166=CARTESIAN_POINT('',(15.2,6.,-19.72));
#20167=CARTESIAN_POINT('Origin',(0.,6.,0.));
#20168=CARTESIAN_POINT('Origin',(14.9979165219706,5.76,-0.74));
#20169=CARTESIAN_POINT('',(-45.17,5.52,-0.5));
#20170=CARTESIAN_POINT('',(-45.17,5.52,-0.5));
#20171=CARTESIAN_POINT('',(-20.4737490231322,5.52,-0.5));
#20172=CARTESIAN_POINT('',(14.9979165219706,5.52,-0.5));
#20173=CARTESIAN_POINT('',(-20.2359894539709,5.74912062451896,-0.729120624518964));
#20174=CARTESIAN_POINT('',(-16.044254314835,9.78854993659521,-4.7685499365952));
#20175=CARTESIAN_POINT('Ctrl Pts',(-20.2359894539709,5.74912062451896,-0.729120624518964));
#20176=CARTESIAN_POINT('Ctrl Pts',(-20.3562758327179,5.87381908208973,-0.853819082089726));
#20177=CARTESIAN_POINT('Ctrl Pts',(-20.4765622114651,6.,-0.98));
#20178=CARTESIAN_POINT('Origin',(15.2,5.76,-19.96));
#20179=CARTESIAN_POINT('',(30.4,5.52,-20.2));
#20180=CARTESIAN_POINT('',(27.8308333333333,2.95083333333333,-22.7691666666667));
#20181=CARTESIAN_POINT('',(22.1531126481133,5.52,-20.2));
#20182=CARTESIAN_POINT('',(15.2,5.52,-20.2));
#20183=CARTESIAN_POINT('Ctrl Pts',(21.9401823146482,6.,-19.72));
#20184=CARTESIAN_POINT('Ctrl Pts',(22.0466474813905,5.76115898072722,-19.9588410192728));
#20185=CARTESIAN_POINT('Ctrl Pts',(22.1531126481134,5.52,-20.2));
#20186=CARTESIAN_POINT('Origin',(30.4,-6.,-20.2));
#20187=CARTESIAN_POINT('',(30.4,-5.52,-20.2));
#20188=CARTESIAN_POINT('',(30.4,-6.,-20.2));
#20189=CARTESIAN_POINT('',(22.1531126481134,-5.52,-20.2));
#20190=CARTESIAN_POINT('',(15.2,-5.52,-20.2));
#20191=CARTESIAN_POINT('',(22.1801713248568,-5.5,-20.2));
#20192=CARTESIAN_POINT('Ctrl Pts',(22.1531126481135,-5.51999999999993,-20.2));
#20193=CARTESIAN_POINT('Ctrl Pts',(22.1666374752019,-5.51000610346768,-20.2));
#20194=CARTESIAN_POINT('Ctrl Pts',(22.1801713248568,-5.5,-20.2));
#20195=CARTESIAN_POINT('',(22.1801713248568,5.5,-20.2));
#20196=CARTESIAN_POINT('',(22.1801713248568,-6.,-20.2));
#20197=CARTESIAN_POINT('Ctrl Pts',(22.1801713248568,5.5,-20.2));
#20198=CARTESIAN_POINT('Ctrl Pts',(22.1666374752019,5.51000610346769,-20.2));
#20199=CARTESIAN_POINT('Ctrl Pts',(22.1531126481135,5.51999999999993,-20.2));
#20200=CARTESIAN_POINT('Origin',(45.65,5.52,-0.98));
#20201=CARTESIAN_POINT('',(45.17,5.52,-0.5));
#20202=CARTESIAN_POINT('',(45.17,5.52,-0.5));
#20203=CARTESIAN_POINT('',(45.65,5.52,-0.98));
#20204=CARTESIAN_POINT('',(45.65,5.52,-0.98));
#20205=CARTESIAN_POINT('',(45.17,6.,-0.98));
#20206=CARTESIAN_POINT('Origin',(45.41,-6.,-0.74));
#20207=CARTESIAN_POINT('',(45.41,-5.76,-0.74));
#20208=CARTESIAN_POINT('',(45.65,-5.52,-0.98));
#20209=CARTESIAN_POINT('',(45.6425,-5.5275,-0.9725));
#20210=CARTESIAN_POINT('',(45.65,-6.,-0.98));
#20211=CARTESIAN_POINT('',(45.17,-5.52,-0.5));
#20212=CARTESIAN_POINT('',(45.17,-6.,-0.5));
#20213=CARTESIAN_POINT('',(40.3813194203284,-0.731319420328439,4.28868057967155));
#20214=CARTESIAN_POINT('Origin',(45.41,5.76,-2.375));
#20215=CARTESIAN_POINT('',(45.65,5.52,-4.));
#20216=CARTESIAN_POINT('',(45.65,5.52,-4.));
#20217=CARTESIAN_POINT('',(45.65,5.52,-2.375));
#20218=CARTESIAN_POINT('Origin',(43.65,5.76,-4.));
#20219=CARTESIAN_POINT('',(43.65,5.52,-6.));
#20220=CARTESIAN_POINT('Origin',(43.65,5.52,-4.));
#20221=CARTESIAN_POINT('',(43.65,5.52,-6.));
#20222=CARTESIAN_POINT('Origin',(22.825,5.76,-5.76));
#20223=CARTESIAN_POINT('',(34.4,5.52,-6.));
#20224=CARTESIAN_POINT('',(32.165,7.755,-3.765));
#20225=CARTESIAN_POINT('',(22.825,5.52,-6.));
#20226=CARTESIAN_POINT('Origin',(14.9979165219706,5.76,-0.74));
#20227=CARTESIAN_POINT('',(20.2359894539709,5.74912062451897,-0.729120624518967));
#20228=CARTESIAN_POINT('',(20.4737490231322,5.52,-0.5));
#20229=CARTESIAN_POINT('',(21.2932340819055,4.73029076090437,0.289709239095628));
#20230=CARTESIAN_POINT('',(14.9979165219706,5.52,-0.5));
#20231=CARTESIAN_POINT('Ctrl Pts',(20.4765622114651,6.,-0.98));
#20232=CARTESIAN_POINT('Ctrl Pts',(20.3562758327179,5.87381908208973,-0.853819082089731));
#20233=CARTESIAN_POINT('Ctrl Pts',(20.2359894539709,5.74912062451897,-0.729120624518967));
#20234=CARTESIAN_POINT('Origin',(43.65,-6.,-4.));
#20235=CARTESIAN_POINT('',(45.65,-5.52,-4.));
#20236=CARTESIAN_POINT('',(45.65,-6.,-4.));
#20237=CARTESIAN_POINT('',(43.65,-5.52,-6.));
#20238=CARTESIAN_POINT('Origin',(43.65,-5.52,-4.));
#20239=CARTESIAN_POINT('',(43.65,-6.,-6.));
#20240=CARTESIAN_POINT('Origin',(45.65,-6.,-0.5));
#20241=CARTESIAN_POINT('',(45.65,-5.52,-2.375));
#20242=CARTESIAN_POINT('Origin',(45.41,-5.76,-2.375));
#20243=CARTESIAN_POINT('',(45.17,-6.,-0.98));
#20244=CARTESIAN_POINT('',(45.17,-6.,-4.));
#20245=CARTESIAN_POINT('Origin',(14.9979165219706,-5.76,-0.74));
#20246=CARTESIAN_POINT('',(20.4737490231322,-5.52,-0.5));
#20247=CARTESIAN_POINT('',(14.9979165219706,-5.52,-0.5));
#20248=CARTESIAN_POINT('',(20.2359894539709,-5.74912062451896,-0.729120624518964));
#20249=CARTESIAN_POINT('',(19.2696493386723,-6.68034897211366,-1.66034897211366));
#20250=CARTESIAN_POINT('Ctrl Pts',(20.2359894539709,-5.74912062451896,-0.729120624518964));
#20251=CARTESIAN_POINT('Ctrl Pts',(20.356275832718,-5.87381908208986,-0.853819082089863));
#20252=CARTESIAN_POINT('Ctrl Pts',(20.4765622114651,-6.,-0.98));
#20253=CARTESIAN_POINT('Origin',(29.9958330439413,-6.,-0.5));
#20254=CARTESIAN_POINT('',(20.4737490231322,-6.,-0.5));
#20255=CARTESIAN_POINT('',(37.25,-2.75545529808154E-16,-0.5));
#20256=CARTESIAN_POINT('Origin',(39.5,0.,-0.5));
#20257=CARTESIAN_POINT('Origin',(20.2248703552884,-6.,-0.7398357130565));
#20258=CARTESIAN_POINT('',(19.9759916874447,5.5,-0.979671426113));
#20259=CARTESIAN_POINT('Ctrl Pts',(20.2359894539709,5.74912062451897,-0.729120624518967));
#20260=CARTESIAN_POINT('Ctrl Pts',(20.1051859468428,5.6229407173369,-0.855171413339672));
#20261=CARTESIAN_POINT('Ctrl Pts',(19.9759916874446,5.5,-0.979671426113002));
#20262=CARTESIAN_POINT('',(19.9759916874447,-5.5,-0.979671426113));
#20263=CARTESIAN_POINT('',(19.9759916874447,-6.,-0.979671426113));
#20264=CARTESIAN_POINT('Ctrl Pts',(19.9759916874447,-5.5,-0.979671426112999));
#20265=CARTESIAN_POINT('Ctrl Pts',(20.1051859468428,-5.62294071733695,-0.855171413339621));
#20266=CARTESIAN_POINT('Ctrl Pts',(20.2359894539709,-5.74912062451896,-0.729120624518964));
#20267=CARTESIAN_POINT('Origin',(43.65,-5.76,-4.));
#20268=CARTESIAN_POINT('',(43.65,-6.,-5.52));
#20269=CARTESIAN_POINT('Origin',(22.825,-5.76,-5.76));
#20270=CARTESIAN_POINT('',(34.4,-5.52,-6.));
#20271=CARTESIAN_POINT('',(22.825,-5.52,-6.));
#20272=CARTESIAN_POINT('',(33.92,-6.,-5.52));
#20273=CARTESIAN_POINT('Origin',(34.16,5.76,-5.125));
#20274=CARTESIAN_POINT('',(34.4,5.52,-34.5));
#20275=CARTESIAN_POINT('',(34.4,5.52,-5.125));
#20276=CARTESIAN_POINT('',(34.4,5.52,-34.5));
#20277=CARTESIAN_POINT('Origin',(34.16,2.,-34.5));
#20278=CARTESIAN_POINT('',(34.4,2.,-38.02));
#20279=CARTESIAN_POINT('',(33.92,2.,-38.5));
#20280=CARTESIAN_POINT('',(34.4,2.,-38.02));
#20281=CARTESIAN_POINT('Origin',(33.92,2.,-34.5));
#20282=CARTESIAN_POINT('Origin',(34.4,2.,-34.5));
#20283=CARTESIAN_POINT('Origin',(34.16,-6.,-38.26));
#20284=CARTESIAN_POINT('',(34.4,-2.,-38.02));
#20285=CARTESIAN_POINT('',(34.4,-6.,-38.02));
#20286=CARTESIAN_POINT('',(33.92,-2.,-38.5));
#20287=CARTESIAN_POINT('',(34.4,-2.,-38.02));
#20288=CARTESIAN_POINT('',(33.92,-6.,-38.5));
#20289=CARTESIAN_POINT('Origin',(34.16,-2.,-34.5));
#20290=CARTESIAN_POINT('',(34.4,-5.52,-34.5));
#20291=CARTESIAN_POINT('',(34.4,-5.52,-34.5));
#20292=CARTESIAN_POINT('Origin',(33.92,-2.,-34.5));
#20293=CARTESIAN_POINT('Origin',(34.4,-2.,-34.5));
#20294=CARTESIAN_POINT('Origin',(34.16,-5.76,-5.125));
#20295=CARTESIAN_POINT('',(34.4,-5.52,-5.125));
#20296=CARTESIAN_POINT('Origin',(45.65,-6.,-6.));
#20297=CARTESIAN_POINT('',(34.4,-6.,-6.));
#20298=CARTESIAN_POINT('',(37.25,-2.75545529808154E-16,-6.));
#20299=CARTESIAN_POINT('Origin',(39.5,0.,-6.));
#20300=CARTESIAN_POINT('Origin',(34.4,-6.,-6.));
#20301=CARTESIAN_POINT('',(34.4,-2.63299061816681E-16,-30.85));
#20302=CARTESIAN_POINT('Origin',(34.4,0.,-33.));
#20303=CARTESIAN_POINT('Origin',(30.64,-5.76,-21.375));
#20304=CARTESIAN_POINT('',(30.4,-5.52,-34.5));
#20305=CARTESIAN_POINT('',(30.4,-5.52,-21.375));
#20306=CARTESIAN_POINT('',(30.4,-5.52,-34.5));
#20307=CARTESIAN_POINT('',(30.88,-6.,-19.72));
#20308=CARTESIAN_POINT('Origin',(15.2,-5.76,-19.96));
#20309=CARTESIAN_POINT('Ctrl Pts',(22.1531126481134,-5.52,-20.2));
#20310=CARTESIAN_POINT('Ctrl Pts',(22.0466474813867,-5.76115898073578,-19.9588410192642));
#20311=CARTESIAN_POINT('Ctrl Pts',(21.9401823146482,-6.,-19.72));
#20312=CARTESIAN_POINT('Origin',(30.64,-2.,-34.5));
#20313=CARTESIAN_POINT('',(30.4,-2.,-38.02));
#20314=CARTESIAN_POINT('',(30.88,-2.,-38.5));
#20315=CARTESIAN_POINT('',(30.4,-2.,-38.02));
#20316=CARTESIAN_POINT('Origin',(30.88,-2.,-34.5));
#20317=CARTESIAN_POINT('Origin',(30.4,-2.,-34.5));
#20318=CARTESIAN_POINT('Origin',(30.64,-6.,-38.26));
#20319=CARTESIAN_POINT('',(30.4,2.,-38.02));
#20320=CARTESIAN_POINT('',(30.88,2.,-38.5));
#20321=CARTESIAN_POINT('',(30.4,2.,-38.02));
#20322=CARTESIAN_POINT('',(30.88,-6.,-38.5));
#20323=CARTESIAN_POINT('',(30.4,-6.,-38.02));
#20324=CARTESIAN_POINT('Origin',(30.64,2.,-34.5));
#20325=CARTESIAN_POINT('',(30.4,5.52,-34.5));
#20326=CARTESIAN_POINT('',(30.4,5.52,-34.5));
#20327=CARTESIAN_POINT('Origin',(30.88,2.,-34.5));
#20328=CARTESIAN_POINT('Origin',(30.4,2.,-34.5));
#20329=CARTESIAN_POINT('Origin',(30.64,5.76,-21.375));
#20330=CARTESIAN_POINT('',(30.4,5.52,-21.375));
#20331=CARTESIAN_POINT('Origin',(30.4,-6.,-38.5));
#20332=CARTESIAN_POINT('',(30.4,-2.63299061816681E-16,-30.85));
#20333=CARTESIAN_POINT('Origin',(30.4,0.,-33.));
#20334=CARTESIAN_POINT('Origin',(-11.0900856624284,-5.76,-19.96));
#20335=CARTESIAN_POINT('Ctrl Pts',(-21.9401823146482,-6.,-19.72));
#20336=CARTESIAN_POINT('Ctrl Pts',(-22.0466474813867,-5.76115898073578,
-19.9588410192642));
#20337=CARTESIAN_POINT('Ctrl Pts',(-22.1531126481134,-5.52,-20.2));
#20338=CARTESIAN_POINT('Origin',(14.9979165219706,-5.76,-0.74));
#20339=CARTESIAN_POINT('',(-20.2359894539709,-5.74912062451896,-0.729120624518966));
#20340=CARTESIAN_POINT('Ctrl Pts',(-20.4765622114651,-6.,-0.98));
#20341=CARTESIAN_POINT('Ctrl Pts',(-20.356275832718,-5.87381908208986,-0.853819082089866));
#20342=CARTESIAN_POINT('Ctrl Pts',(-20.2359894539709,-5.74912062451896,
-0.729120624518966));
#20343=CARTESIAN_POINT('',(-20.4737490231322,-5.52,-0.5));
#20344=CARTESIAN_POINT('',(-14.0206695716018,-11.7386081478045,-6.71860814780449));
#20345=CARTESIAN_POINT('',(-45.17,-5.52,-0.5));
#20346=CARTESIAN_POINT('',(14.9979165219706,-5.52,-0.5));
#20347=CARTESIAN_POINT('',(-45.17,-5.52,-0.5));
#20348=CARTESIAN_POINT('Origin',(-45.41,-6.,-0.74));
#20349=CARTESIAN_POINT('',(-45.17,-6.,-0.5));
#20350=CARTESIAN_POINT('',(-45.65,-6.,-0.98));
#20351=CARTESIAN_POINT('Origin',(0.,-5.75,0.));
#20352=CARTESIAN_POINT('',(-19.9759916874447,-5.5,-0.979671426113));
#20353=CARTESIAN_POINT('Origin',(0.,-5.5,0.));
#20354=CARTESIAN_POINT('Ctrl Pts',(-20.2359894539709,-5.74912062451896,
-0.729120624518967));
#20355=CARTESIAN_POINT('Ctrl Pts',(-20.1051859468429,-5.62294071733704,
-0.855171413339538));
#20356=CARTESIAN_POINT('Ctrl Pts',(-19.9759916874447,-5.5,-0.979671426112999));
#20357=CARTESIAN_POINT('Origin',(-45.65,-6.,-6.));
#20358=CARTESIAN_POINT('',(-45.65,-6.,-4.));
#20359=CARTESIAN_POINT('Origin',(0.,5.75,0.));
#20360=CARTESIAN_POINT('',(-19.9759916874447,5.5,-0.979671426113));
#20361=CARTESIAN_POINT('Ctrl Pts',(-19.9759916874447,5.5,-0.979671426113));
#20362=CARTESIAN_POINT('Ctrl Pts',(-20.1051859468429,5.62294071733699,-0.85517141333958));
#20363=CARTESIAN_POINT('Ctrl Pts',(-20.2359894539709,5.74912062451896,-0.729120624518964));
#20364=CARTESIAN_POINT('Origin',(0.,5.5,0.));
#20365=CARTESIAN_POINT('Origin',(0.,-6.,0.));
#20366=CARTESIAN_POINT('',(-19.9759916874447,-6.,-0.979671426113));
#20367=CARTESIAN_POINT('',(4.91078361144855,-3.48,-19.3877333466687));
#20368=CARTESIAN_POINT('',(4.91078361144856,3.48,-19.3877333466687));
#20369=CARTESIAN_POINT('',(4.91078361144855,-6.,-19.3877333466687));
#20370=CARTESIAN_POINT('',(-4.91078361144855,-3.48,-19.3877333466687));
#20371=CARTESIAN_POINT('Origin',(0.,-3.48,0.));
#20372=CARTESIAN_POINT('',(-4.91078361144855,3.48,-19.3877333466687));
#20373=CARTESIAN_POINT('',(-4.91078361144855,-6.,-19.3877333466687));
#20374=CARTESIAN_POINT('Origin',(0.,3.48,0.));
#20375=CARTESIAN_POINT('Origin',(-20.2248703552884,-6.,-0.7398357130565));
#20376=CARTESIAN_POINT('',(-20.4737490231322,-6.,-0.5));
#20377=CARTESIAN_POINT('Origin',(-4.91744041005317,-6.,-19.4438666733343));
#20378=CARTESIAN_POINT('',(-4.92409720865779,-3.36789585050059,-19.5));
#20379=CARTESIAN_POINT('Ctrl Pts',(-4.91078361144855,-3.48,-19.3877333466687));
#20380=CARTESIAN_POINT('Ctrl Pts',(-4.91522154689806,-3.44263314413296,
-19.4251561523001));
#20381=CARTESIAN_POINT('Ctrl Pts',(-4.91965948264541,-3.40526449477787,
-19.4625789604431));
#20382=CARTESIAN_POINT('Ctrl Pts',(-4.92409720865779,-3.36789585050059,
-19.5));
#20383=CARTESIAN_POINT('',(-4.92409720865779,3.36789585050059,-19.5));
#20384=CARTESIAN_POINT('',(-4.92409720865779,-6.,-19.5));
#20385=CARTESIAN_POINT('Ctrl Pts',(-4.92409720865779,3.36789585050059,-19.5));
#20386=CARTESIAN_POINT('Ctrl Pts',(-4.91965948264339,3.40526449479487,-19.4625789604261));
#20387=CARTESIAN_POINT('Ctrl Pts',(-4.91522154689707,3.44263314414129,-19.4251561522918));
#20388=CARTESIAN_POINT('Ctrl Pts',(-4.91078361144855,3.48,-19.3877333466687));
#20389=CARTESIAN_POINT('Origin',(4.91744041005317,-6.,-19.4438666733343));
#20390=CARTESIAN_POINT('',(4.92409720865779,3.36789585050059,-19.5));
#20391=CARTESIAN_POINT('Ctrl Pts',(4.91078361144855,3.48,-19.3877333466687));
#20392=CARTESIAN_POINT('Ctrl Pts',(4.9152215468944,3.44263314416375,-19.4251561522693));
#20393=CARTESIAN_POINT('Ctrl Pts',(4.91965948263797,3.4052644948405,-19.4625789603804));
#20394=CARTESIAN_POINT('Ctrl Pts',(4.92409720865779,3.36789585050059,-19.5));
#20395=CARTESIAN_POINT('',(4.92409720865779,-3.36789585050059,-19.5));
#20396=CARTESIAN_POINT('',(4.92409720865779,-6.,-19.5));
#20397=CARTESIAN_POINT('Ctrl Pts',(4.92409720865779,-3.36789585050059,-19.5));
#20398=CARTESIAN_POINT('Ctrl Pts',(4.91965948264544,-3.40526449477763,-19.4625789604433));
#20399=CARTESIAN_POINT('Ctrl Pts',(4.91522154689809,-3.44263314413272,-19.4251561523004));
#20400=CARTESIAN_POINT('Ctrl Pts',(4.91078361144855,-3.48,-19.3877333466687));
#20401=CARTESIAN_POINT('Origin',(0.,3.24,0.));
#20402=CARTESIAN_POINT('',(-6.25942489371028,3.,-19.5));
#20403=CARTESIAN_POINT('',(6.25942489371028,3.,-19.5));
#20404=CARTESIAN_POINT('Origin',(0.,3.,0.));
#20405=CARTESIAN_POINT('Ctrl Pts',(6.25942489371028,3.00000000000001,-19.5));
#20406=CARTESIAN_POINT('Ctrl Pts',(5.58570985570301,3.20591155664892,-19.5));
#20407=CARTESIAN_POINT('Ctrl Pts',(4.92409720865779,3.36789585050059,-19.5));
#20408=CARTESIAN_POINT('Ctrl Pts',(-4.92409720865779,3.3678958505006,-19.5));
#20409=CARTESIAN_POINT('Ctrl Pts',(-5.58570985570301,3.20591155664892,-19.5));
#20410=CARTESIAN_POINT('Ctrl Pts',(-6.25942489371029,3.,-19.5));
#20411=CARTESIAN_POINT('Origin',(0.,-3.24,0.));
#20412=CARTESIAN_POINT('',(6.25942489371028,-3.,-19.5));
#20413=CARTESIAN_POINT('Ctrl Pts',(4.92409720865779,-3.36789585050059,-19.5));
#20414=CARTESIAN_POINT('Ctrl Pts',(5.58570985570301,-3.20591155664891,-19.5));
#20415=CARTESIAN_POINT('Ctrl Pts',(6.25942489371028,-3.,-19.5));
#20416=CARTESIAN_POINT('',(-6.25942489371028,-3.,-19.5));
#20417=CARTESIAN_POINT('Origin',(0.,-3.,0.));
#20418=CARTESIAN_POINT('Ctrl Pts',(-6.25942489371028,-3.,-19.5));
#20419=CARTESIAN_POINT('Ctrl Pts',(-5.58570985570301,-3.20591155664891,
-19.5));
#20420=CARTESIAN_POINT('Ctrl Pts',(-4.92409720865778,-3.36789585050059,
-19.5));
#20421=CARTESIAN_POINT('Origin',(0.,-3.,-25.25));
#20422=CARTESIAN_POINT('',(11.,-3.,-19.5));
#20423=CARTESIAN_POINT('',(11.,-3.,-19.5));
#20424=CARTESIAN_POINT('',(11.,-3.,-27.3939847411799));
#20425=CARTESIAN_POINT('',(11.,-3.,-31.));
#20426=CARTESIAN_POINT('',(-11.,-3.,-27.3939847411799));
#20427=CARTESIAN_POINT('Origin',(0.,-3.,0.));
#20428=CARTESIAN_POINT('',(-11.,-3.,-19.5));
#20429=CARTESIAN_POINT('',(-11.,-3.,-19.5));
#20430=CARTESIAN_POINT('',(11.,-3.,-19.5));
#20431=CARTESIAN_POINT('Origin',(-11.,-3.,-19.5));
#20432=CARTESIAN_POINT('',(11.,3.,-19.5));
#20433=CARTESIAN_POINT('',(11.,3.,-19.5));
#20434=CARTESIAN_POINT('',(11.,-3.,-19.5));
#20435=CARTESIAN_POINT('Origin',(-11.2225734265705,-6.,-27.5807880133765));
#20436=CARTESIAN_POINT('',(-11.445146853141,-3.48,-27.7310045528473));
#20437=CARTESIAN_POINT('',(-11.445146853141,3.48,-27.7310045528473));
#20438=CARTESIAN_POINT('',(-11.445146853141,-6.,-27.7310045528473));
#20439=CARTESIAN_POINT('',(-11.,3.03395491952051,-27.4305714739057));
#20440=CARTESIAN_POINT('Ctrl Pts',(-11.445146853141,3.48,-27.7310045528473));
#20441=CARTESIAN_POINT('Ctrl Pts',(-11.2969785213058,3.33103640993591,-27.6310045914395));
#20442=CARTESIAN_POINT('Ctrl Pts',(-11.14857662724,3.1823261888354,-27.5308469970628));
#20443=CARTESIAN_POINT('Ctrl Pts',(-11.,3.03395491952051,-27.4305714739057));
#20444=CARTESIAN_POINT('',(-11.,-3.03395491952051,-27.4305714739057));
#20445=CARTESIAN_POINT('',(-11.,-6.,-27.4305714739057));
#20446=CARTESIAN_POINT('Ctrl Pts',(-11.,-3.03395491952051,-27.4305714739057));
#20447=CARTESIAN_POINT('Ctrl Pts',(-11.14857662724,-3.18232618883539,-27.5308469970628));
#20448=CARTESIAN_POINT('Ctrl Pts',(-11.2969785213057,-3.33103640993588,
-27.6310045914395));
#20449=CARTESIAN_POINT('Ctrl Pts',(-11.445146853141,-3.48,-27.7310045528473));
#20450=CARTESIAN_POINT('Origin',(11.2225734265705,-6.,-27.5807880133765));
#20451=CARTESIAN_POINT('',(11.445146853141,3.48,-27.7310045528473));
#20452=CARTESIAN_POINT('',(11.445146853141,-3.48,-27.7310045528473));
#20453=CARTESIAN_POINT('',(11.445146853141,-6.,-27.7310045528473));
#20454=CARTESIAN_POINT('',(11.,-3.03395491952051,-27.4305714739057));
#20455=CARTESIAN_POINT('Ctrl Pts',(11.445146853141,-3.48,-27.7310045528473));
#20456=CARTESIAN_POINT('Ctrl Pts',(11.2969785213068,-3.33103640993696,-27.6310045914402));
#20457=CARTESIAN_POINT('Ctrl Pts',(11.1485766272405,-3.1823261888359,-27.5308469970632));
#20458=CARTESIAN_POINT('Ctrl Pts',(11.,-3.03395491952051,-27.4305714739057));
#20459=CARTESIAN_POINT('',(11.,3.03395491952051,-27.4305714739057));
#20460=CARTESIAN_POINT('',(11.,-6.,-27.4305714739057));
#20461=CARTESIAN_POINT('Ctrl Pts',(11.,3.03395491952051,-27.4305714739057));
#20462=CARTESIAN_POINT('Ctrl Pts',(11.1485766272405,3.18232618883592,-27.5308469970632));
#20463=CARTESIAN_POINT('Ctrl Pts',(11.2969785213068,3.33103640993699,-27.6310045914402));
#20464=CARTESIAN_POINT('Ctrl Pts',(11.445146853141,3.48,-27.7310045528473));
#20465=CARTESIAN_POINT('Origin',(0.,-3.24,0.));
#20466=CARTESIAN_POINT('Ctrl Pts',(11.,-3.,-27.39398474118));
#20467=CARTESIAN_POINT('Ctrl Pts',(11.,-3.01696612998714,-27.4122675927604));
#20468=CARTESIAN_POINT('Ctrl Pts',(11.,-3.0339549195205,-27.4305714739057));
#20469=CARTESIAN_POINT('Origin',(0.,-3.48,0.));
#20470=CARTESIAN_POINT('Ctrl Pts',(-11.,-3.0339549195205,-27.4305714739057));
#20471=CARTESIAN_POINT('Ctrl Pts',(-11.,-3.01696612998714,-27.4122675927604));
#20472=CARTESIAN_POINT('Ctrl Pts',(-11.,-2.99999999999999,-27.3939847411799));
#20473=CARTESIAN_POINT('Origin',(0.,3.24,0.));
#20474=CARTESIAN_POINT('Origin',(0.,3.48,0.));
#20475=CARTESIAN_POINT('',(11.,3.,-27.3939847411799));
#20476=CARTESIAN_POINT('Ctrl Pts',(11.,3.03395491952051,-27.4305714739057));
#20477=CARTESIAN_POINT('Ctrl Pts',(11.,3.01696612998715,-27.4122675927604));
#20478=CARTESIAN_POINT('Ctrl Pts',(11.,3.,-27.3939847411799));
#20479=CARTESIAN_POINT('',(-11.,3.,-27.3939847411799));
#20480=CARTESIAN_POINT('Origin',(0.,3.,0.));
#20481=CARTESIAN_POINT('Ctrl Pts',(-11.,3.,-27.3939847411799));
#20482=CARTESIAN_POINT('Ctrl Pts',(-11.,3.01696612998714,-27.4122675927604));
#20483=CARTESIAN_POINT('Ctrl Pts',(-11.,3.03395491952051,-27.4305714739057));
#20484=CARTESIAN_POINT('Origin',(0.,3.,-25.25));
#20485=CARTESIAN_POINT('',(-11.,3.,-19.5));
#20486=CARTESIAN_POINT('',(11.,3.,-19.5));
#20487=CARTESIAN_POINT('',(-11.,3.,-19.5));
#20488=CARTESIAN_POINT('',(11.,3.,-31.));
#20489=CARTESIAN_POINT('Origin',(11.,-3.,-19.5));
#20490=CARTESIAN_POINT('Origin',(0.,-6.,0.));
#20491=CARTESIAN_POINT('Origin',(0.,5.5,0.));
#20492=CARTESIAN_POINT('Origin',(0.,-5.5,0.));
#20493=CARTESIAN_POINT('Origin',(0.,5.75,0.));
#20494=CARTESIAN_POINT('Origin',(29.9958330439413,-6.,-0.5));
#20495=CARTESIAN_POINT('',(-41.75,-2.75545529808155E-16,-0.5));
#20496=CARTESIAN_POINT('Origin',(-39.5,0.,-0.5));
#20497=CARTESIAN_POINT('Origin',(0.,-5.75,0.));
#20498=CARTESIAN_POINT('Origin',(-11.,-3.,-31.));
#20499=CARTESIAN_POINT('',(-11.,-3.,-19.5));
#20500=CARTESIAN_POINT('Origin',(-11.,-3.,-19.5));
#20501=CARTESIAN_POINT('Origin',(39.5,0.,-0.5));
#20502=CARTESIAN_POINT('',(37.25,2.75545529808154E-16,-0.5));
#20503=CARTESIAN_POINT('Origin',(-39.5,0.,-0.5));
#20504=CARTESIAN_POINT('',(-41.75,-2.75545529808155E-16,-6.));
#20505=CARTESIAN_POINT('',(-41.75,2.75545529808155E-16,-0.5));
#20506=CARTESIAN_POINT('Origin',(-39.5,0.,-6.));
#20507=CARTESIAN_POINT('Origin',(-34.4,0.,-33.));
#20508=CARTESIAN_POINT('',(-34.4,-2.63299061816681E-16,-30.85));
#20509=CARTESIAN_POINT('Origin',(-34.4,0.,-33.));
#20510=CARTESIAN_POINT('',(-34.4,-2.63299061816681E-16,-30.85));
#20511=CARTESIAN_POINT('Origin',(34.4,0.,-33.));
#20512=CARTESIAN_POINT('',(34.4,2.63299061816681E-16,-30.85));
#20513=CARTESIAN_POINT('Origin',(17.2,-2.,-34.5));
#20514=CARTESIAN_POINT('',(17.2,-2.,-38.5));
#20515=CARTESIAN_POINT('Origin',(17.2,2.,-34.5));
#20516=CARTESIAN_POINT('',(17.2,2.,-38.5));
#20517=CARTESIAN_POINT('Origin',(-43.65,-6.,-4.));
#20518=CARTESIAN_POINT('',(-43.65,-6.,-6.));
#20519=CARTESIAN_POINT('Origin',(-34.4,-6.,-6.));
#20520=CARTESIAN_POINT('',(-34.4,-6.,-6.));
#20521=CARTESIAN_POINT('Origin',(34.4,-6.,-38.5));
#20522=CARTESIAN_POINT('Origin',(-34.4,-6.,-38.5));
#20523=CARTESIAN_POINT('',(0.,0.,0.));
#20524=CARTESIAN_POINT('Origin',(29.95,5.75,-36.75));
#20525=CARTESIAN_POINT('',(30.2,5.5,-40.));
#20526=CARTESIAN_POINT('',(29.7,6.,-40.));
#20527=CARTESIAN_POINT('',(25.275,10.425,-40.));
#20528=CARTESIAN_POINT('',(29.7,6.,-33.));
#20529=CARTESIAN_POINT('',(29.7,6.,-36.75));
#20530=CARTESIAN_POINT('',(30.2,5.5,-33.));
#20531=CARTESIAN_POINT('',(29.7,6.,-33.));
#20532=CARTESIAN_POINT('',(30.2,5.5,-36.75));
#20533=CARTESIAN_POINT('Origin',(29.95,5.55111512312578E-16,-33.));
#20534=CARTESIAN_POINT('',(29.7,-6.,-33.));
#20535=CARTESIAN_POINT('',(30.2,-5.5,-33.));
#20536=CARTESIAN_POINT('',(29.7,-6.,-33.));
#20537=CARTESIAN_POINT('Origin',(30.2,5.55111512312578E-16,-33.));
#20538=CARTESIAN_POINT('Origin',(29.7,5.55111512312578E-16,-33.));
#20539=CARTESIAN_POINT('Origin',(29.95,-5.75,-33.25));
#20540=CARTESIAN_POINT('',(29.7,-6.,-40.));
#20541=CARTESIAN_POINT('',(30.2,-5.5,-40.));
#20542=CARTESIAN_POINT('',(24.525,-11.175,-40.));
#20543=CARTESIAN_POINT('',(30.2,-5.5,-33.25));
#20544=CARTESIAN_POINT('',(29.7,-6.,-33.25));
#20545=CARTESIAN_POINT('Origin',(25.2,-6.,-33.));
#20546=CARTESIAN_POINT('',(25.7,-6.,-33.));
#20547=CARTESIAN_POINT('',(25.2,-6.,-33.));
#20548=CARTESIAN_POINT('',(25.7,-6.,-40.));
#20549=CARTESIAN_POINT('',(25.7,-6.,-33.25));
#20550=CARTESIAN_POINT('',(14.6,-6.,-40.));
#20551=CARTESIAN_POINT('Origin',(25.2,5.55111512312578E-16,-33.));
#20552=CARTESIAN_POINT('',(25.7,6.,-33.));
#20553=CARTESIAN_POINT('',(25.2,6.,-33.));
#20554=CARTESIAN_POINT('Origin',(25.7,5.55111512312578E-16,-33.));
#20555=CARTESIAN_POINT('Origin',(25.2,6.,-40.));
#20556=CARTESIAN_POINT('',(25.7,6.,-40.));
#20557=CARTESIAN_POINT('',(14.6,6.,-40.));
#20558=CARTESIAN_POINT('',(25.7,6.,-36.75));
#20559=CARTESIAN_POINT('Origin',(25.45,5.75,-36.75));
#20560=CARTESIAN_POINT('',(25.2,5.5,-40.));
#20561=CARTESIAN_POINT('',(18.275,-1.42500000000001,-40.));
#20562=CARTESIAN_POINT('',(25.2,5.5,-33.));
#20563=CARTESIAN_POINT('',(25.2,5.5,-36.75));
#20564=CARTESIAN_POINT('',(25.2,5.5,-33.));
#20565=CARTESIAN_POINT('Origin',(25.45,5.55111512312578E-16,-33.));
#20566=CARTESIAN_POINT('',(25.2,-5.5,-33.));
#20567=CARTESIAN_POINT('',(25.2,-5.5,-33.));
#20568=CARTESIAN_POINT('Origin',(25.2,5.55111512312578E-16,-33.));
#20569=CARTESIAN_POINT('Origin',(25.45,-5.75,-33.25));
#20570=CARTESIAN_POINT('',(25.2,-5.5,-40.));
#20571=CARTESIAN_POINT('',(19.025,0.675000000000006,-40.));
#20572=CARTESIAN_POINT('',(25.2,-5.5,-33.25));
#20573=CARTESIAN_POINT('Origin',(25.2,0.,-33.5));
#20574=CARTESIAN_POINT('',(25.2,-0.75,-40.));
#20575=CARTESIAN_POINT('',(25.2,4.05,-35.338268590218));
#20576=CARTESIAN_POINT('',(25.2,2.77555756156289E-15,-37.676537180436));
#20577=CARTESIAN_POINT('',(25.2,1.02924682452695,-37.0823012492328));
#20578=CARTESIAN_POINT('',(25.2,4.05,-30.661731409782));
#20579=CARTESIAN_POINT('',(25.2,4.05,-34.2747967278116));
#20580=CARTESIAN_POINT('',(25.2,5.55111512312578E-16,-28.323462819564));
#20581=CARTESIAN_POINT('',(25.2,3.02075317547306,-30.0674954785788));
#20582=CARTESIAN_POINT('',(25.2,-4.05,-30.661731409782));
#20583=CARTESIAN_POINT('',(25.2,-1.24575317547306,-29.0426987507672));
#20584=CARTESIAN_POINT('',(25.2,-4.05,-35.338268590218));
#20585=CARTESIAN_POINT('',(25.2,-4.05,-32.2252032721884));
#20586=CARTESIAN_POINT('',(25.2,-2.80424682452695,-36.0575045214212));
#20587=CARTESIAN_POINT('Origin',(-29.95,-5.75,-36.75));
#20588=CARTESIAN_POINT('',(-30.2,-5.5,-40.));
#20589=CARTESIAN_POINT('',(-29.7,-6.,-40.));
#20590=CARTESIAN_POINT('',(-22.525,-13.175,-40.));
#20591=CARTESIAN_POINT('',(-29.7,-6.,-33.));
#20592=CARTESIAN_POINT('',(-29.7,-6.,-36.75));
#20593=CARTESIAN_POINT('',(-30.2,-5.5,-33.));
#20594=CARTESIAN_POINT('',(-29.7,-6.,-33.));
#20595=CARTESIAN_POINT('',(-30.2,-5.5,-36.75));
#20596=CARTESIAN_POINT('Origin',(-29.95,5.55111512312578E-16,-33.));
#20597=CARTESIAN_POINT('',(-29.7,6.,-33.));
#20598=CARTESIAN_POINT('',(-30.2,5.5,-33.));
#20599=CARTESIAN_POINT('',(-29.7,6.,-33.));
#20600=CARTESIAN_POINT('Origin',(-30.2,5.55111512312578E-16,-33.));
#20601=CARTESIAN_POINT('Origin',(-29.7,5.55111512312578E-16,-33.));
#20602=CARTESIAN_POINT('Origin',(-29.95,5.75,-33.25));
#20603=CARTESIAN_POINT('',(-29.7,6.,-40.));
#20604=CARTESIAN_POINT('',(-30.2,5.5,-40.));
#20605=CARTESIAN_POINT('',(-23.275,12.425,-40.));
#20606=CARTESIAN_POINT('',(-30.2,5.5,-33.25));
#20607=CARTESIAN_POINT('',(-29.7,6.,-33.25));
#20608=CARTESIAN_POINT('Origin',(-25.2,6.,-33.));
#20609=CARTESIAN_POINT('',(-25.7,6.,-33.));
#20610=CARTESIAN_POINT('',(-25.2,6.,-33.));
#20611=CARTESIAN_POINT('',(-25.7,6.,-40.));
#20612=CARTESIAN_POINT('',(-25.7,6.,-33.25));
#20613=CARTESIAN_POINT('',(-10.6,6.,-40.));
#20614=CARTESIAN_POINT('Origin',(-25.2,5.55111512312578E-16,-33.));
#20615=CARTESIAN_POINT('',(-25.7,-6.,-33.));
#20616=CARTESIAN_POINT('',(-25.2,-6.,-33.));
#20617=CARTESIAN_POINT('Origin',(-25.7,5.55111512312578E-16,-33.));
#20618=CARTESIAN_POINT('Origin',(-25.2,-6.,-40.));
#20619=CARTESIAN_POINT('',(-25.7,-6.,-40.));
#20620=CARTESIAN_POINT('',(-10.6,-6.,-40.));
#20621=CARTESIAN_POINT('',(-25.7,-6.,-36.75));
#20622=CARTESIAN_POINT('Origin',(22.,2.5,-38.));
#20623=CARTESIAN_POINT('',(21.5,2.,-38.));
#20624=CARTESIAN_POINT('',(21.5,2.5,-37.5));
#20625=CARTESIAN_POINT('',(21.5,2.,-38.));
#20626=CARTESIAN_POINT('',(22.,2.5,-38.));
#20627=CARTESIAN_POINT('',(22.,2.5,-38.));
#20628=CARTESIAN_POINT('',(21.5,2.5,-37.5));
#20629=CARTESIAN_POINT('Origin',(21.75,2.25,-40.));
#20630=CARTESIAN_POINT('',(21.5,2.,-40.));
#20631=CARTESIAN_POINT('',(22.,2.5,-40.));
#20632=CARTESIAN_POINT('',(16.375,-3.12500000000001,-40.));
#20633=CARTESIAN_POINT('',(22.,2.5,-40.));
#20634=CARTESIAN_POINT('',(21.5,2.,-40.));
#20635=CARTESIAN_POINT('Origin',(21.75,3.5,-37.75));
#20636=CARTESIAN_POINT('',(21.75,7.75,-37.75));
#20637=CARTESIAN_POINT('',(21.5,7.5,-37.5));
#20638=CARTESIAN_POINT('',(22.6666666666667,8.66666666666666,-38.6666666666667));
#20639=CARTESIAN_POINT('',(21.5,3.5,-37.5));
#20640=CARTESIAN_POINT('',(22.,7.5,-38.));
#20641=CARTESIAN_POINT('',(22.,3.5,-38.));
#20642=CARTESIAN_POINT('',(24.0833333333333,5.41666666666666,-40.0833333333333));
#20643=CARTESIAN_POINT('Origin',(16.,2.25,-37.75));
#20644=CARTESIAN_POINT('',(14.25,2.25,-37.75));
#20645=CARTESIAN_POINT('',(14.5,2.,-38.));
#20646=CARTESIAN_POINT('',(14.9166666666667,1.58333333333333,-38.4166666666667));
#20647=CARTESIAN_POINT('',(16.,2.,-38.));
#20648=CARTESIAN_POINT('',(14.5,2.5,-37.5));
#20649=CARTESIAN_POINT('',(16.,2.5,-37.5));
#20650=CARTESIAN_POINT('',(15.25,3.25,-36.75));
#20651=CARTESIAN_POINT('Origin',(22.,2.,-40.));
#20652=CARTESIAN_POINT('',(22.,7.5,-40.));
#20653=CARTESIAN_POINT('',(22.,0.25,-40.));
#20654=CARTESIAN_POINT('',(22.,7.5,-47.5));
#20655=CARTESIAN_POINT('Origin',(14.,2.,-40.));
#20656=CARTESIAN_POINT('',(14.5,2.,-40.));
#20657=CARTESIAN_POINT('',(14.5,2.,-40.));
#20658=CARTESIAN_POINT('',(9.,2.,-40.));
#20659=CARTESIAN_POINT('Origin',(14.25,2.25,-40.));
#20660=CARTESIAN_POINT('',(14.,2.5,-38.));
#20661=CARTESIAN_POINT('',(14.5,2.,-37.5));
#20662=CARTESIAN_POINT('',(14.,2.5,-40.));
#20663=CARTESIAN_POINT('',(14.,2.5,-40.));
#20664=CARTESIAN_POINT('',(12.625,3.875,-40.));
#20665=CARTESIAN_POINT('Origin',(29.95,0.,-33.));
#20666=CARTESIAN_POINT('',(30.2,-3.24531401774048E-16,-30.35));
#20667=CARTESIAN_POINT('Origin',(30.2,0.,-33.));
#20668=CARTESIAN_POINT('',(29.7,2.63299061816681E-16,-30.85));
#20669=CARTESIAN_POINT('',(29.95,-2.93915231795365E-16,-30.6));
#20670=CARTESIAN_POINT('Origin',(29.7,0.,-33.));
#20671=CARTESIAN_POINT('Origin',(30.2,0.,-33.));
#20672=CARTESIAN_POINT('',(28.9,-2.63299061816681E-16,-30.85));
#20673=CARTESIAN_POINT('',(30.2,2.63299061816681E-16,-30.85));
#20674=CARTESIAN_POINT('Origin',(28.9,0.,-33.));
#20675=CARTESIAN_POINT('Origin',(30.2,0.,-33.5));
#20676=CARTESIAN_POINT('',(30.2,-0.75,-40.));
#20677=CARTESIAN_POINT('Origin',(-29.95,0.,-33.));
#20678=CARTESIAN_POINT('',(-30.2,3.24531401774048E-16,-30.35));
#20679=CARTESIAN_POINT('Origin',(-30.2,0.,-33.));
#20680=CARTESIAN_POINT('',(-29.7,-2.63299061816681E-16,-30.85));
#20681=CARTESIAN_POINT('',(-29.95,2.93915231795365E-16,-30.6));
#20682=CARTESIAN_POINT('Origin',(-29.7,0.,-33.));
#20683=CARTESIAN_POINT('Origin',(-30.2,0.,-33.));
#20684=CARTESIAN_POINT('',(-28.9,2.63299061816681E-16,-30.85));
#20685=CARTESIAN_POINT('',(-30.2,-2.63299061816681E-16,-30.85));
#20686=CARTESIAN_POINT('Origin',(-28.9,0.,-33.));
#20687=CARTESIAN_POINT('Origin',(-30.2,0.,-33.5));
#20688=CARTESIAN_POINT('',(-30.2,-0.75,-40.));
#20689=CARTESIAN_POINT('Origin',(28.65,0.,-33.));
#20690=CARTESIAN_POINT('',(28.4,3.24531401774048E-16,-30.35));
#20691=CARTESIAN_POINT('',(28.65,-2.93915231795365E-16,-30.6));
#20692=CARTESIAN_POINT('Origin',(28.4,0.,-33.));
#20693=CARTESIAN_POINT('Origin',(28.4,0.,-33.));
#20694=CARTESIAN_POINT('',(28.4,3.55,-35.0495934556232));
#20695=CARTESIAN_POINT('',(28.4,3.55,-30.9504065443768));
#20696=CARTESIAN_POINT('',(28.4,3.55,-35.0495934556232));
#20697=CARTESIAN_POINT('',(28.4,-5.55111512312578E-16,-37.0991869112463));
#20698=CARTESIAN_POINT('',(28.4,-7.53008419494684E-16,-37.0991869112463));
#20699=CARTESIAN_POINT('',(28.4,-3.55,-35.0495934556232));
#20700=CARTESIAN_POINT('',(28.4,-3.55,-35.0495934556232));
#20701=CARTESIAN_POINT('',(28.4,-3.55,-30.9504065443768));
#20702=CARTESIAN_POINT('',(28.4,-3.55,-30.9504065443768));
#20703=CARTESIAN_POINT('',(28.4,0.,-28.9008130887537));
#20704=CARTESIAN_POINT('',(28.4,2.51002806498228E-16,-28.9008130887537));
#20705=CARTESIAN_POINT('',(28.4,3.55,-30.9504065443768));
#20706=CARTESIAN_POINT('Origin',(25.45,-1.12075317547306,-29.2592051017133));
#20707=CARTESIAN_POINT('',(25.7,2.51002806498228E-16,-28.9008130887537));
#20708=CARTESIAN_POINT('',(25.2,5.55111512312578E-16,-28.323462819564));
#20709=CARTESIAN_POINT('',(25.7,-3.55,-30.9504065443768));
#20710=CARTESIAN_POINT('',(25.7,-0.995753175473055,-29.4757114526594));
#20711=CARTESIAN_POINT('',(25.2,-4.05,-30.661731409782));
#20712=CARTESIAN_POINT('Origin',(25.45,2.89575317547306,-30.2840018295249));
#20713=CARTESIAN_POINT('',(25.7,3.55,-30.9504065443768));
#20714=CARTESIAN_POINT('',(25.2,4.05,-30.661731409782));
#20715=CARTESIAN_POINT('',(25.7,2.77075317547306,-30.500508180471));
#20716=CARTESIAN_POINT('Origin',(25.45,0.904246824526946,-36.8657948982867));
#20717=CARTESIAN_POINT('',(25.7,-7.53008419494684E-16,-37.0991869112463));
#20718=CARTESIAN_POINT('',(25.2,2.77555756156289E-15,-37.676537180436));
#20719=CARTESIAN_POINT('',(25.7,3.55,-35.0495934556232));
#20720=CARTESIAN_POINT('',(25.7,0.779246824526944,-36.6492885473405));
#20721=CARTESIAN_POINT('',(25.7,3.55,-35.0495934556232));
#20722=CARTESIAN_POINT('Origin',(25.45,-2.67924682452694,-35.8409981704751));
#20723=CARTESIAN_POINT('',(25.7,-3.55,-35.0495934556232));
#20724=CARTESIAN_POINT('',(25.7,-2.55424682452694,-35.624491819529));
#20725=CARTESIAN_POINT('',(25.2,-4.05,-35.338268590218));
#20726=CARTESIAN_POINT('Origin',(25.45,3.8,-34.2747967278116));
#20727=CARTESIAN_POINT('',(25.7,3.55,-34.2747967278116));
#20728=CARTESIAN_POINT('Origin',(25.45,-3.8,-32.2252032721884));
#20729=CARTESIAN_POINT('',(25.7,-3.55,-32.2252032721884));
#20730=CARTESIAN_POINT('Origin',(25.2,3.55,-30.9504065443768));
#20731=CARTESIAN_POINT('',(25.2,3.55,-30.9504065443768));
#20732=CARTESIAN_POINT('',(25.2,2.51002806498228E-16,-28.9008130887537));
#20733=CARTESIAN_POINT('Origin',(25.2,3.55,-35.0495934556232));
#20734=CARTESIAN_POINT('',(25.2,3.55,-35.0495934556232));
#20735=CARTESIAN_POINT('Origin',(25.2,-7.53008419494684E-16,-37.0991869112463));
#20736=CARTESIAN_POINT('',(25.2,-7.53008419494684E-16,-37.0991869112463));
#20737=CARTESIAN_POINT('Origin',(-28.65,0.,-33.));
#20738=CARTESIAN_POINT('',(-28.4,-3.24531401774048E-16,-30.35));
#20739=CARTESIAN_POINT('',(-28.65,2.93915231795365E-16,-30.6));
#20740=CARTESIAN_POINT('Origin',(-28.4,0.,-33.));
#20741=CARTESIAN_POINT('Origin',(-28.4,0.,-33.));
#20742=CARTESIAN_POINT('',(-28.4,3.55,-30.9504065443768));
#20743=CARTESIAN_POINT('',(-28.4,3.55,-35.0495934556232));
#20744=CARTESIAN_POINT('',(-28.4,3.55,-35.0495934556232));
#20745=CARTESIAN_POINT('',(-28.4,0.,-28.9008130887537));
#20746=CARTESIAN_POINT('',(-28.4,3.55,-30.9504065443768));
#20747=CARTESIAN_POINT('',(-28.4,-3.55,-30.9504065443768));
#20748=CARTESIAN_POINT('',(-28.4,2.51002806498228E-16,-28.9008130887537));
#20749=CARTESIAN_POINT('',(-28.4,-3.55,-35.0495934556232));
#20750=CARTESIAN_POINT('',(-28.4,-3.55,-30.9504065443768));
#20751=CARTESIAN_POINT('',(-28.4,-5.55111512312578E-16,-37.0991869112463));
#20752=CARTESIAN_POINT('',(-28.4,-3.55,-35.0495934556232));
#20753=CARTESIAN_POINT('',(-28.4,-7.53008419494684E-16,-37.0991869112463));
#20754=CARTESIAN_POINT('Origin',(-25.45,5.75,-33.25));
#20755=CARTESIAN_POINT('',(-25.2,5.5,-40.));
#20756=CARTESIAN_POINT('',(-16.275,-3.42500000000001,-40.));
#20757=CARTESIAN_POINT('',(-25.2,5.5,-33.));
#20758=CARTESIAN_POINT('',(-25.7,6.,-33.));
#20759=CARTESIAN_POINT('',(-25.2,5.5,-33.25));
#20760=CARTESIAN_POINT('Origin',(-25.45,5.55111512312578E-16,-33.));
#20761=CARTESIAN_POINT('',(-25.2,-5.5,-33.));
#20762=CARTESIAN_POINT('',(-25.7,-6.,-33.));
#20763=CARTESIAN_POINT('Origin',(-25.2,5.55111512312578E-16,-33.));
#20764=CARTESIAN_POINT('Origin',(-25.45,-5.75,-36.75));
#20765=CARTESIAN_POINT('',(-25.2,-5.5,-40.));
#20766=CARTESIAN_POINT('',(-17.025,2.675,-40.));
#20767=CARTESIAN_POINT('',(-25.2,-5.5,-36.75));
#20768=CARTESIAN_POINT('Origin',(-25.45,-0.904246824526945,-36.8657948982867));
#20769=CARTESIAN_POINT('',(-25.2,-4.05,-35.338268590218));
#20770=CARTESIAN_POINT('',(-25.2,2.22044604925031E-15,-37.676537180436));
#20771=CARTESIAN_POINT('',(-25.2,-1.02924682452694,-37.0823012492328));
#20772=CARTESIAN_POINT('',(-25.7,-7.53008419494684E-16,-37.0991869112463));
#20773=CARTESIAN_POINT('',(-25.2,2.22044604925031E-15,-37.676537180436));
#20774=CARTESIAN_POINT('',(-25.7,-3.55,-35.0495934556232));
#20775=CARTESIAN_POINT('',(-25.7,-0.779246824526944,-36.6492885473405));
#20776=CARTESIAN_POINT('',(-25.2,-4.05,-35.338268590218));
#20777=CARTESIAN_POINT('Origin',(-25.45,2.67924682452694,-35.8409981704751));
#20778=CARTESIAN_POINT('',(-25.2,4.05,-35.338268590218));
#20779=CARTESIAN_POINT('',(-25.2,2.80424682452694,-36.0575045214212));
#20780=CARTESIAN_POINT('',(-25.7,3.55,-35.0495934556232));
#20781=CARTESIAN_POINT('',(-25.2,4.05,-35.338268590218));
#20782=CARTESIAN_POINT('',(-25.7,2.55424682452694,-35.624491819529));
#20783=CARTESIAN_POINT('Origin',(-25.45,1.12075317547306,-29.2592051017133));
#20784=CARTESIAN_POINT('',(-25.2,4.05,-30.661731409782));
#20785=CARTESIAN_POINT('',(-25.2,0.,-28.323462819564));
#20786=CARTESIAN_POINT('',(-25.2,1.24575317547306,-29.0426987507672));
#20787=CARTESIAN_POINT('',(-25.7,2.51002806498228E-16,-28.9008130887537));
#20788=CARTESIAN_POINT('',(-25.2,0.,-28.323462819564));
#20789=CARTESIAN_POINT('',(-25.7,3.55,-30.9504065443768));
#20790=CARTESIAN_POINT('',(-25.7,0.995753175473055,-29.4757114526594));
#20791=CARTESIAN_POINT('',(-25.7,3.55,-30.9504065443768));
#20792=CARTESIAN_POINT('Origin',(-25.45,-2.89575317547306,-30.2840018295249));
#20793=CARTESIAN_POINT('',(-25.7,-3.55,-30.9504065443768));
#20794=CARTESIAN_POINT('',(-25.7,-2.77075317547306,-30.500508180471));
#20795=CARTESIAN_POINT('',(-25.2,-4.05,-30.661731409782));
#20796=CARTESIAN_POINT('',(-25.2,-3.02075317547306,-30.0674954785788));
#20797=CARTESIAN_POINT('',(-25.2,-4.05,-30.661731409782));
#20798=CARTESIAN_POINT('Origin',(-25.45,3.8,-32.2252032721884));
#20799=CARTESIAN_POINT('',(-25.2,4.05,-32.2252032721884));
#20800=CARTESIAN_POINT('',(-25.7,3.55,-32.2252032721884));
#20801=CARTESIAN_POINT('Origin',(-25.45,-3.8,-34.2747967278116));
#20802=CARTESIAN_POINT('',(-25.7,-3.55,-34.2747967278116));
#20803=CARTESIAN_POINT('',(-25.2,-4.05,-34.2747967278116));
#20804=CARTESIAN_POINT('Origin',(-25.2,3.55,-35.0495934556232));
#20805=CARTESIAN_POINT('',(-25.2,3.55,-35.0495934556232));
#20806=CARTESIAN_POINT('',(-25.2,-7.53008419494684E-16,-37.0991869112463));
#20807=CARTESIAN_POINT('Origin',(-25.2,3.55,-30.9504065443768));
#20808=CARTESIAN_POINT('',(-25.2,3.55,-30.9504065443768));
#20809=CARTESIAN_POINT('Origin',(-25.2,0.,-28.9008130887537));
#20810=CARTESIAN_POINT('',(-25.2,2.51002806498228E-16,-28.9008130887537));
#20811=CARTESIAN_POINT('Origin',(-25.2,0.,-33.5));
#20812=CARTESIAN_POINT('',(-25.2,-0.75,-40.));
#20813=CARTESIAN_POINT('Origin',(-23.5,2.,-38.));
#20814=CARTESIAN_POINT('',(-24.,2.5,-38.));
#20815=CARTESIAN_POINT('',(-23.5,2.5,-37.5));
#20816=CARTESIAN_POINT('',(-24.,2.5,-38.));
#20817=CARTESIAN_POINT('',(-23.5,2.,-38.));
#20818=CARTESIAN_POINT('',(-23.5,2.,-38.));
#20819=CARTESIAN_POINT('',(-23.5,2.5,-37.5));
#20820=CARTESIAN_POINT('Origin',(-23.75,2.25,-40.));
#20821=CARTESIAN_POINT('',(-24.,2.5,-40.));
#20822=CARTESIAN_POINT('',(-23.5,2.,-40.));
#20823=CARTESIAN_POINT('',(-15.875,-5.625,-40.));
#20824=CARTESIAN_POINT('',(-23.5,2.,-40.));
#20825=CARTESIAN_POINT('',(-24.,2.5,-40.));
#20826=CARTESIAN_POINT('Origin',(-16.,2.5,-38.));
#20827=CARTESIAN_POINT('',(-16.5,2.,-38.));
#20828=CARTESIAN_POINT('',(-16.5,2.5,-37.5));
#20829=CARTESIAN_POINT('',(-16.5,2.,-38.));
#20830=CARTESIAN_POINT('',(-16.,2.5,-38.));
#20831=CARTESIAN_POINT('',(-16.,2.5,-38.));
#20832=CARTESIAN_POINT('',(-16.5,2.5,-37.5));
#20833=CARTESIAN_POINT('Origin',(-16.25,2.25,-40.));
#20834=CARTESIAN_POINT('',(-16.5,2.,-40.));
#20835=CARTESIAN_POINT('',(-16.,2.5,-40.));
#20836=CARTESIAN_POINT('',(-12.125,6.375,-40.));
#20837=CARTESIAN_POINT('',(-16.,2.5,-40.));
#20838=CARTESIAN_POINT('',(-16.5,2.,-40.));
#20839=CARTESIAN_POINT('Origin',(-16.25,3.5,-37.75));
#20840=CARTESIAN_POINT('',(-16.25,7.75,-37.75));
#20841=CARTESIAN_POINT('',(-16.5,7.5,-37.5));
#20842=CARTESIAN_POINT('',(-12.1666666666666,11.8333333333333,-41.8333333333334));
#20843=CARTESIAN_POINT('',(-16.5,3.5,-37.5));
#20844=CARTESIAN_POINT('',(-16.,7.5,-38.));
#20845=CARTESIAN_POINT('',(-16.,3.5,-38.));
#20846=CARTESIAN_POINT('',(-13.9166666666667,5.41666666666667,-40.0833333333333));
#20847=CARTESIAN_POINT('Origin',(-22.,2.25,-37.75));
#20848=CARTESIAN_POINT('',(-22.,2.5,-37.5));
#20849=CARTESIAN_POINT('',(-22.,2.,-38.));
#20850=CARTESIAN_POINT('Origin',(-23.75,6.5,-37.75));
#20851=CARTESIAN_POINT('',(-23.75,7.75,-37.75));
#20852=CARTESIAN_POINT('',(-24.,7.5,-38.));
#20853=CARTESIAN_POINT('',(-25.5833333333333,5.91666666666667,-39.5833333333333));
#20854=CARTESIAN_POINT('',(-24.,6.5,-38.));
#20855=CARTESIAN_POINT('',(-23.5,7.5,-37.5));
#20856=CARTESIAN_POINT('',(-23.5,6.5,-37.5));
#20857=CARTESIAN_POINT('',(-17.5,1.50000000000001,-31.5));
#20858=CARTESIAN_POINT('Origin',(-24.,2.,-40.));
#20859=CARTESIAN_POINT('',(-10.,2.,-40.));
#20860=CARTESIAN_POINT('Origin',(-24.,8.,-40.));
#20861=CARTESIAN_POINT('',(-24.,7.5,-40.));
#20862=CARTESIAN_POINT('',(-24.,7.5,-47.5));
#20863=CARTESIAN_POINT('',(-24.,3.25,-40.));
#20864=CARTESIAN_POINT('Origin',(-23.75,7.75,-47.5));
#20865=CARTESIAN_POINT('',(-23.5,8.,-38.));
#20866=CARTESIAN_POINT('',(-24.,7.5,-37.5));
#20867=CARTESIAN_POINT('',(-23.5,8.,-40.5));
#20868=CARTESIAN_POINT('',(-23.5,8.,-47.5));
#20869=CARTESIAN_POINT('',(-24.,7.5,-40.));
#20870=CARTESIAN_POINT('Origin',(-3.5,2.,-38.));
#20871=CARTESIAN_POINT('',(-4.,2.5,-38.));
#20872=CARTESIAN_POINT('',(-3.5,2.5,-37.5));
#20873=CARTESIAN_POINT('',(-4.,2.5,-38.));
#20874=CARTESIAN_POINT('',(-3.5,2.,-38.));
#20875=CARTESIAN_POINT('',(-3.5,2.,-38.));
#20876=CARTESIAN_POINT('',(-3.5,2.5,-37.5));
#20877=CARTESIAN_POINT('Origin',(-3.75,2.25,-40.));
#20878=CARTESIAN_POINT('',(-4.,2.5,-40.));
#20879=CARTESIAN_POINT('',(-3.5,2.,-40.));
#20880=CARTESIAN_POINT('',(-0.874999999999997,-0.624999999999997,-40.));
#20881=CARTESIAN_POINT('',(-3.5,2.,-40.));
#20882=CARTESIAN_POINT('',(-4.,2.5,-40.));
#20883=CARTESIAN_POINT('Origin',(4.,2.5,-38.));
#20884=CARTESIAN_POINT('',(3.5,2.,-38.));
#20885=CARTESIAN_POINT('',(3.5,2.5,-37.5));
#20886=CARTESIAN_POINT('',(3.5,2.,-38.));
#20887=CARTESIAN_POINT('',(4.,2.5,-38.));
#20888=CARTESIAN_POINT('',(4.,2.5,-38.));
#20889=CARTESIAN_POINT('',(3.5,2.5,-37.5));
#20890=CARTESIAN_POINT('Origin',(3.75,2.25,-40.));
#20891=CARTESIAN_POINT('',(3.5,2.,-40.));
#20892=CARTESIAN_POINT('',(4.,2.5,-40.));
#20893=CARTESIAN_POINT('',(2.875,1.375,-40.));
#20894=CARTESIAN_POINT('',(4.,2.5,-40.));
#20895=CARTESIAN_POINT('',(3.5,2.,-40.));
#20896=CARTESIAN_POINT('Origin',(3.75,3.5,-37.75));
#20897=CARTESIAN_POINT('',(3.75,7.75,-37.75));
#20898=CARTESIAN_POINT('',(3.5,7.5,-37.5));
#20899=CARTESIAN_POINT('',(6.16666666666669,10.1666666666667,-40.1666666666667));
#20900=CARTESIAN_POINT('',(3.5,3.5,-37.5));
#20901=CARTESIAN_POINT('',(4.,7.5,-38.));
#20902=CARTESIAN_POINT('',(4.,3.5,-38.));
#20903=CARTESIAN_POINT('',(6.08333333333334,5.41666666666668,-40.0833333333333));
#20904=CARTESIAN_POINT('Origin',(-2.,2.25,-37.75));
#20905=CARTESIAN_POINT('',(-2.,2.5,-37.5));
#20906=CARTESIAN_POINT('',(-2.,2.,-38.));
#20907=CARTESIAN_POINT('Origin',(-3.75,6.5,-37.75));
#20908=CARTESIAN_POINT('',(-3.75,7.75,-37.75));
#20909=CARTESIAN_POINT('',(-4.,7.5,-38.));
#20910=CARTESIAN_POINT('',(-5.58333333333333,5.91666666666667,-39.5833333333333));
#20911=CARTESIAN_POINT('',(-4.,6.5,-38.));
#20912=CARTESIAN_POINT('',(-3.5,7.5,-37.5));
#20913=CARTESIAN_POINT('',(-3.5,6.5,-37.5));
#20914=CARTESIAN_POINT('',(0.833333333333363,3.16666666666667,-33.1666666666667));
#20915=CARTESIAN_POINT('Origin',(-4.,2.,-40.));
#20916=CARTESIAN_POINT('',(-2.77555756156289E-15,2.,-40.));
#20917=CARTESIAN_POINT('Origin',(-4.,8.,-40.));
#20918=CARTESIAN_POINT('',(-4.,7.5,-40.));
#20919=CARTESIAN_POINT('',(-4.,7.5,-47.5));
#20920=CARTESIAN_POINT('',(-4.,3.25,-40.));
#20921=CARTESIAN_POINT('Origin',(-3.75,7.75,-47.5));
#20922=CARTESIAN_POINT('',(-3.5,8.,-38.));
#20923=CARTESIAN_POINT('',(-4.,7.5,-37.5));
#20924=CARTESIAN_POINT('',(-3.5,8.,-40.5));
#20925=CARTESIAN_POINT('',(-3.5,8.,-47.5));
#20926=CARTESIAN_POINT('',(-4.,7.5,-40.));
#20927=CARTESIAN_POINT('Origin',(14.25,6.5,-37.75));
#20928=CARTESIAN_POINT('',(14.5,7.5,-37.5));
#20929=CARTESIAN_POINT('',(14.5,6.5,-37.5));
#20930=CARTESIAN_POINT('',(14.25,7.75,-37.75));
#20931=CARTESIAN_POINT('',(17.3333333333334,4.66666666666667,-34.6666666666667));
#20932=CARTESIAN_POINT('',(14.,7.5,-38.));
#20933=CARTESIAN_POINT('',(12.4166666666667,5.91666666666667,-39.5833333333333));
#20934=CARTESIAN_POINT('',(14.,6.5,-38.));
#20935=CARTESIAN_POINT('Origin',(14.,8.,-40.));
#20936=CARTESIAN_POINT('',(14.,7.5,-40.));
#20937=CARTESIAN_POINT('',(14.,7.5,-47.5));
#20938=CARTESIAN_POINT('',(14.,3.25,-40.));
#20939=CARTESIAN_POINT('Origin',(14.25,7.75,-47.5));
#20940=CARTESIAN_POINT('',(14.5,8.,-38.));
#20941=CARTESIAN_POINT('',(14.,7.5,-37.5));
#20942=CARTESIAN_POINT('',(14.5,8.,-40.5));
#20943=CARTESIAN_POINT('',(14.5,8.,-47.5));
#20944=CARTESIAN_POINT('',(14.,7.5,-40.));
#20945=CARTESIAN_POINT('Origin',(6.75,7.75,-53.25));
#20946=CARTESIAN_POINT('',(-31.5,7.5,-53.));
#20947=CARTESIAN_POINT('',(39.5,7.5,-53.));
#20948=CARTESIAN_POINT('',(6.75,7.5,-53.));
#20949=CARTESIAN_POINT('',(40.,8.,-53.5));
#20950=CARTESIAN_POINT('',(34.3750000000001,2.37500000000007,-47.875));
#20951=CARTESIAN_POINT('',(-32.,8.,-53.5));
#20952=CARTESIAN_POINT('',(6.75,8.,-53.5));
#20953=CARTESIAN_POINT('',(-32.,8.,-53.5));
#20954=CARTESIAN_POINT('Origin',(-31.75,7.75,-48.5));
#20955=CARTESIAN_POINT('',(-32.,8.,-41.5));
#20956=CARTESIAN_POINT('',(-32.,8.,-48.5));
#20957=CARTESIAN_POINT('',(-31.5,7.5,-42.));
#20958=CARTESIAN_POINT('',(-18.2916666666667,-5.70833333333324,-55.2083333333334));
#20959=CARTESIAN_POINT('',(-31.5,7.5,-48.5));
#20960=CARTESIAN_POINT('Origin',(-31.5,8.,-53.));
#20961=CARTESIAN_POINT('',(-31.5,-9.,-53.));
#20962=CARTESIAN_POINT('',(-31.5,8.,-53.));
#20963=CARTESIAN_POINT('',(39.5,-9.,-53.));
#20964=CARTESIAN_POINT('',(-31.5,-9.,-53.));
#20965=CARTESIAN_POINT('',(39.5,8.,-53.));
#20966=CARTESIAN_POINT('Origin',(-31.5,8.,-42.));
#20967=CARTESIAN_POINT('',(-31.5,-9.,-42.));
#20968=CARTESIAN_POINT('',(-31.5,8.,-42.));
#20969=CARTESIAN_POINT('',(-31.5,-9.,-42.));
#20970=CARTESIAN_POINT('Origin',(39.75,7.75,-54.));
#20971=CARTESIAN_POINT('',(40.,8.,-41.5));
#20972=CARTESIAN_POINT('',(40.,8.,-54.));
#20973=CARTESIAN_POINT('',(39.5,7.5,-42.));
#20974=CARTESIAN_POINT('',(39.5,7.5,-54.));
#20975=CARTESIAN_POINT('',(39.5,7.5,-42.));
#20976=CARTESIAN_POINT('Origin',(42.25,7.75,-41.75));
#20977=CARTESIAN_POINT('',(42.25,7.5,-42.));
#20978=CARTESIAN_POINT('',(42.25,8.,-41.5));
#20979=CARTESIAN_POINT('Origin',(45.,8.,-55.));
#20980=CARTESIAN_POINT('',(-35.5,8.,-54.5));
#20981=CARTESIAN_POINT('',(43.5,8.,-54.5));
#20982=CARTESIAN_POINT('',(24.5,8.,-54.5));
#20983=CARTESIAN_POINT('',(-35.5,8.,-48.7951833846989));
#20984=CARTESIAN_POINT('',(-35.5,8.,-55.));
#20985=CARTESIAN_POINT('',(-35.5,8.,-46.2048166153011));
#20986=CARTESIAN_POINT('Origin',(-34.25,8.,-47.5));
#20987=CARTESIAN_POINT('',(-35.5,8.,-40.5));
#20988=CARTESIAN_POINT('',(-35.5,8.,-55.));
#20989=CARTESIAN_POINT('',(24.5,8.,-40.5));
#20990=CARTESIAN_POINT('',(-16.5,8.,-38.));
#20991=CARTESIAN_POINT('',(12.5,8.,-38.));
#20992=CARTESIAN_POINT('',(-16.5,8.,-40.5));
#20993=CARTESIAN_POINT('',(-16.5,8.,-47.5));
#20994=CARTESIAN_POINT('',(24.5,8.,-40.5));
#20995=CARTESIAN_POINT('',(3.5,8.,-38.));
#20996=CARTESIAN_POINT('',(22.5,8.,-38.));
#20997=CARTESIAN_POINT('',(3.5,8.,-40.5));
#20998=CARTESIAN_POINT('',(3.5,8.,-47.5));
#20999=CARTESIAN_POINT('',(24.5,8.,-40.5));
#21000=CARTESIAN_POINT('',(21.5,8.,-38.));
#21001=CARTESIAN_POINT('',(31.5,8.,-38.));
#21002=CARTESIAN_POINT('',(21.5,8.,-40.5));
#21003=CARTESIAN_POINT('',(21.5,8.,-47.5));
#21004=CARTESIAN_POINT('',(43.5,8.,-40.5));
#21005=CARTESIAN_POINT('',(24.5,8.,-40.5));
#21006=CARTESIAN_POINT('',(43.5,8.,-46.2048166153011));
#21007=CARTESIAN_POINT('',(43.5,8.,-55.));
#21008=CARTESIAN_POINT('',(43.5,8.,-48.7951833846989));
#21009=CARTESIAN_POINT('Origin',(42.25,8.,-47.5));
#21010=CARTESIAN_POINT('',(43.5,8.,-55.));
#21011=CARTESIAN_POINT('Origin',(24.5,7.75,-54.75));
#21012=CARTESIAN_POINT('',(-35.5,7.5,-55.));
#21013=CARTESIAN_POINT('',(-35.5,7.5,-55.));
#21014=CARTESIAN_POINT('',(43.5,7.5,-55.));
#21015=CARTESIAN_POINT('',(43.5,8.,-54.5));
#21016=CARTESIAN_POINT('',(24.5,7.5,-55.));
#21017=CARTESIAN_POINT('Origin',(-35.5,6.5,-54.75));
#21018=CARTESIAN_POINT('',(-36.5,6.5,-55.));
#21019=CARTESIAN_POINT('',(-37.,6.5,-54.5));
#21020=CARTESIAN_POINT('',(-36.5,6.5,-55.));
#21021=CARTESIAN_POINT('Origin',(-35.5,6.5,-54.5));
#21022=CARTESIAN_POINT('Origin',(-35.5,6.5,-55.));
#21023=CARTESIAN_POINT('Origin',(-36.75,3.25,-54.75));
#21024=CARTESIAN_POINT('',(-36.5,-9.5,-55.));
#21025=CARTESIAN_POINT('',(-37.,-9.5,-54.5));
#21026=CARTESIAN_POINT('',(-36.5,-9.5,-55.));
#21027=CARTESIAN_POINT('',(-37.,3.25,-54.5));
#21028=CARTESIAN_POINT('',(-36.5,3.25,-55.));
#21029=CARTESIAN_POINT('Origin',(-35.5,-9.5,-54.75));
#21030=CARTESIAN_POINT('',(-35.5,-10.5,-55.));
#21031=CARTESIAN_POINT('',(-35.5,-11.,-54.5));
#21032=CARTESIAN_POINT('',(-35.5,-10.5,-55.));
#21033=CARTESIAN_POINT('Origin',(-35.5,-9.5,-54.5));
#21034=CARTESIAN_POINT('Origin',(-35.5,-9.5,-55.));
#21035=CARTESIAN_POINT('Origin',(-16.5,-10.75,-54.75));
#21036=CARTESIAN_POINT('',(43.5,-10.5,-55.));
#21037=CARTESIAN_POINT('',(43.5,-11.,-54.5));
#21038=CARTESIAN_POINT('',(43.5,-10.5,-55.));
#21039=CARTESIAN_POINT('',(-16.5,-11.,-54.5));
#21040=CARTESIAN_POINT('',(-16.5,-10.5,-55.));
#21041=CARTESIAN_POINT('Origin',(43.5,-9.5,-54.75));
#21042=CARTESIAN_POINT('',(44.5,-9.5,-55.));
#21043=CARTESIAN_POINT('',(45.,-9.5,-54.5));
#21044=CARTESIAN_POINT('',(44.5,-9.5,-55.));
#21045=CARTESIAN_POINT('Origin',(43.5,-9.5,-54.5));
#21046=CARTESIAN_POINT('Origin',(43.5,-9.5,-55.));
#21047=CARTESIAN_POINT('Origin',(44.75,-6.25,-54.75));
#21048=CARTESIAN_POINT('',(44.5,6.5,-55.));
#21049=CARTESIAN_POINT('',(45.,6.5,-54.5));
#21050=CARTESIAN_POINT('',(44.5,6.5,-55.));
#21051=CARTESIAN_POINT('',(45.,-6.25,-54.5));
#21052=CARTESIAN_POINT('',(44.5,-6.25,-55.));
#21053=CARTESIAN_POINT('Origin',(43.5,6.5,-54.75));
#21054=CARTESIAN_POINT('Origin',(43.5,6.5,-54.5));
#21055=CARTESIAN_POINT('Origin',(43.5,6.5,-55.));
#21056=CARTESIAN_POINT('Origin',(43.5,-9.5,-55.));
#21057=CARTESIAN_POINT('',(45.,-9.5,-40.5));
#21058=CARTESIAN_POINT('',(45.,-9.5,-55.));
#21059=CARTESIAN_POINT('',(43.5,-11.,-40.5));
#21060=CARTESIAN_POINT('Origin',(43.5,-9.5,-40.5));
#21061=CARTESIAN_POINT('',(43.5,-11.,-55.));
#21062=CARTESIAN_POINT('Origin',(45.,-11.,-55.));
#21063=CARTESIAN_POINT('',(45.,6.5,-40.5));
#21064=CARTESIAN_POINT('',(45.,6.5,-55.));
#21065=CARTESIAN_POINT('',(45.,-6.25,-40.5));
#21066=CARTESIAN_POINT('',(45.,-3.,-44.5));
#21067=CARTESIAN_POINT('Origin',(45.,-3.,-47.5));
#21068=CARTESIAN_POINT('Origin',(43.5,6.5,-55.));
#21069=CARTESIAN_POINT('',(43.9750046174461,7.92280378598205,-47.9927598805759));
#21070=CARTESIAN_POINT('Ctrl Pts',(43.9750046174461,7.92280378598205,-47.9927598805759));
#21071=CARTESIAN_POINT('Ctrl Pts',(43.8929060558365,7.95021248156921,-48.295755755381));
#21072=CARTESIAN_POINT('Ctrl Pts',(43.7266147755088,8.,-48.5764742252605));
#21073=CARTESIAN_POINT('Ctrl Pts',(43.5,8.,-48.7951833846989));
#21074=CARTESIAN_POINT('',(43.9750046174461,7.92280378598205,-47.0072401194241));
#21075=CARTESIAN_POINT('Ctrl Pts',(43.9750046174461,7.92280378598205,-47.0072401194241));
#21076=CARTESIAN_POINT('Ctrl Pts',(44.0191184364596,7.90807633871839,-47.1700481506604));
#21077=CARTESIAN_POINT('Ctrl Pts',(44.0399563324054,7.89944521405426,-47.3379114457046));
#21078=CARTESIAN_POINT('Ctrl Pts',(44.0399563324054,7.89944521405426,-47.6620885542954));
#21079=CARTESIAN_POINT('Ctrl Pts',(44.0191184364596,7.9080763387184,-47.8299518493397));
#21080=CARTESIAN_POINT('Ctrl Pts',(43.9750046174461,7.92280378598205,-47.9927598805759));
#21081=CARTESIAN_POINT('Ctrl Pts',(43.5,8.,-46.2048166153011));
#21082=CARTESIAN_POINT('Ctrl Pts',(43.7266147755088,8.,-46.4235257747395));
#21083=CARTESIAN_POINT('Ctrl Pts',(43.8929060558365,7.95021248156921,-46.704244244619));
#21084=CARTESIAN_POINT('Ctrl Pts',(43.9750046174461,7.92280378598205,-47.0072401194241));
#21085=CARTESIAN_POINT('Origin',(43.5,6.5,-40.5));
#21086=CARTESIAN_POINT('Origin',(3.99999999999999,-1.5,-55.));
#21087=CARTESIAN_POINT('Origin',(24.5,7.75,-40.25));
#21088=CARTESIAN_POINT('',(4.,7.5,-40.));
#21089=CARTESIAN_POINT('',(24.5,7.5,-40.));
#21090=CARTESIAN_POINT('',(3.5,8.,-40.5));
#21091=CARTESIAN_POINT('Origin',(24.5,7.75,-40.25));
#21092=CARTESIAN_POINT('',(-16.,7.5,-40.));
#21093=CARTESIAN_POINT('',(-16.5,8.,-40.5));
#21094=CARTESIAN_POINT('',(24.5,7.5,-40.));
#21095=CARTESIAN_POINT('Origin',(-16.25,7.75,-47.5));
#21096=CARTESIAN_POINT('',(-16.,7.5,-47.5));
#21097=CARTESIAN_POINT('',(-16.5,8.,-38.));
#21098=CARTESIAN_POINT('Origin',(24.5,7.75,-40.25));
#21099=CARTESIAN_POINT('',(-35.5,7.5,-40.));
#21100=CARTESIAN_POINT('',(-35.5,8.,-40.5));
#21101=CARTESIAN_POINT('',(24.5,7.5,-40.));
#21102=CARTESIAN_POINT('Origin',(-35.5,6.5,-40.25));
#21103=CARTESIAN_POINT('',(-37.,6.5,-40.5));
#21104=CARTESIAN_POINT('Origin',(-35.5,6.5,-40.5));
#21105=CARTESIAN_POINT('',(-36.5,6.5,-40.));
#21106=CARTESIAN_POINT('',(-37.,6.5,-40.5));
#21107=CARTESIAN_POINT('Origin',(-35.5,6.5,-40.));
#21108=CARTESIAN_POINT('Origin',(-36.75,3.25,-40.25));
#21109=CARTESIAN_POINT('',(-37.,-9.5,-40.5));
#21110=CARTESIAN_POINT('',(-36.5,-9.5,-40.));
#21111=CARTESIAN_POINT('',(-37.,-9.5,-40.5));
#21112=CARTESIAN_POINT('',(-36.5,3.25,-40.));
#21113=CARTESIAN_POINT('',(-37.,3.25,-40.5));
#21114=CARTESIAN_POINT('Origin',(-35.5,-9.5,-40.25));
#21115=CARTESIAN_POINT('',(-35.5,-11.,-40.5));
#21116=CARTESIAN_POINT('Origin',(-35.5,-9.5,-40.5));
#21117=CARTESIAN_POINT('',(-35.5,-10.5,-40.));
#21118=CARTESIAN_POINT('',(-35.5,-11.,-40.5));
#21119=CARTESIAN_POINT('Origin',(-35.5,-9.5,-40.));
#21120=CARTESIAN_POINT('Origin',(-16.5,-10.75,-40.25));
#21121=CARTESIAN_POINT('',(43.5,-10.5,-40.));
#21122=CARTESIAN_POINT('',(43.5,-11.,-40.5));
#21123=CARTESIAN_POINT('',(-16.5,-10.5,-40.));
#21124=CARTESIAN_POINT('',(-16.5,-11.,-40.5));
#21125=CARTESIAN_POINT('Origin',(43.5,-9.5,-40.25));
#21126=CARTESIAN_POINT('',(44.5,-9.5,-40.));
#21127=CARTESIAN_POINT('',(45.,-9.5,-40.5));
#21128=CARTESIAN_POINT('Origin',(43.5,-9.5,-40.));
#21129=CARTESIAN_POINT('Origin',(44.75,-6.25,-40.25));
#21130=CARTESIAN_POINT('',(44.5,6.5,-40.));
#21131=CARTESIAN_POINT('',(45.,6.5,-40.5));
#21132=CARTESIAN_POINT('',(44.5,-6.25,-40.));
#21133=CARTESIAN_POINT('Origin',(43.5,6.5,-40.25));
#21134=CARTESIAN_POINT('',(43.5,7.5,-40.));
#21135=CARTESIAN_POINT('',(43.5,8.,-40.5));
#21136=CARTESIAN_POINT('Origin',(43.5,6.5,-40.));
#21137=CARTESIAN_POINT('Origin',(24.5,7.75,-40.25));
#21138=CARTESIAN_POINT('',(24.5,7.5,-40.));
#21139=CARTESIAN_POINT('',(21.5,8.,-40.5));
#21140=CARTESIAN_POINT('Origin',(21.75,7.75,-47.5));
#21141=CARTESIAN_POINT('',(21.5,8.,-38.));
#21142=CARTESIAN_POINT('Origin',(12.5,7.75,-37.75));
#21143=CARTESIAN_POINT('',(12.5,7.5,-37.5));
#21144=CARTESIAN_POINT('Origin',(31.5,7.75,-37.75));
#21145=CARTESIAN_POINT('',(31.5,7.5,-37.5));
#21146=CARTESIAN_POINT('Origin',(3.75,7.75,-47.5));
#21147=CARTESIAN_POINT('',(4.,7.5,-47.5));
#21148=CARTESIAN_POINT('',(3.5,8.,-38.));
#21149=CARTESIAN_POINT('Origin',(22.5,7.75,-37.75));
#21150=CARTESIAN_POINT('',(22.5,7.5,-37.5));
#21151=CARTESIAN_POINT('Origin',(-37.,-11.,-55.));
#21152=CARTESIAN_POINT('',(-35.5,-11.,-55.));
#21153=CARTESIAN_POINT('Origin',(-35.5,-9.5,-55.));
#21154=CARTESIAN_POINT('',(-37.,-9.5,-55.));
#21155=CARTESIAN_POINT('Origin',(-37.,8.,-55.));
#21156=CARTESIAN_POINT('',(-37.,6.5,-55.));
#21157=CARTESIAN_POINT('Origin',(-35.5,6.5,-55.));
#21158=CARTESIAN_POINT('',(-35.9750046174461,7.92280378598206,-47.0072401194241));
#21159=CARTESIAN_POINT('Ctrl Pts',(-35.9750046174461,7.92280378598206,-47.0072401194241));
#21160=CARTESIAN_POINT('Ctrl Pts',(-35.8929060558365,7.95021248156921,-46.704244244619));
#21161=CARTESIAN_POINT('Ctrl Pts',(-35.7266147755088,8.,-46.4235257747395));
#21162=CARTESIAN_POINT('Ctrl Pts',(-35.5,8.,-46.2048166153011));
#21163=CARTESIAN_POINT('',(-35.9750046174461,7.92280378598205,-47.9927598805758));
#21164=CARTESIAN_POINT('Ctrl Pts',(-35.9750046174461,7.92280378598205,-47.9927598805758));
#21165=CARTESIAN_POINT('Ctrl Pts',(-36.0191184364596,7.90807633871838,-47.8299518493395));
#21166=CARTESIAN_POINT('Ctrl Pts',(-36.0399563352666,7.8994452073828,-47.662088554661));
#21167=CARTESIAN_POINT('Ctrl Pts',(-36.0399563352666,7.8994452073828,-47.337911445339));
#21168=CARTESIAN_POINT('Ctrl Pts',(-36.0191184364596,7.90807633871839,-47.1700481506605));
#21169=CARTESIAN_POINT('Ctrl Pts',(-35.9750046174461,7.92280378598206,-47.0072401194241));
#21170=CARTESIAN_POINT('Ctrl Pts',(-35.5,8.,-48.7951833846989));
#21171=CARTESIAN_POINT('Ctrl Pts',(-35.7266147755088,8.,-48.5764742252605));
#21172=CARTESIAN_POINT('Ctrl Pts',(-35.8929060558365,7.95021248156921,-48.295755755381));
#21173=CARTESIAN_POINT('Ctrl Pts',(-35.9750046174461,7.92280378598205,-47.9927598805758));
#21174=CARTESIAN_POINT('Origin',(4.,2.,-40.));
#21175=CARTESIAN_POINT('',(4.,0.25,-40.));
#21176=CARTESIAN_POINT('Origin',(0.,5.,-37.5));
#21177=CARTESIAN_POINT('Origin',(3.99999999999999,-1.5,-40.));
#21178=CARTESIAN_POINT('',(-16.,0.25,-40.));
#21179=CARTESIAN_POINT('Origin',(-16.,2.,-40.));
#21180=CARTESIAN_POINT('Origin',(-20.,5.,-37.5));
#21181=CARTESIAN_POINT('Ctrl Pts',(43.9750046174461,7.92280378598205,-47.9927598805759));
#21182=CARTESIAN_POINT('Ctrl Pts',(44.0191184364596,7.9080763387184,-47.8299518493397));
#21183=CARTESIAN_POINT('Ctrl Pts',(44.0399563324054,7.89944521405426,-47.6620885542954));
#21184=CARTESIAN_POINT('Ctrl Pts',(44.0399563324054,7.89944521405426,-47.3379114457046));
#21185=CARTESIAN_POINT('Ctrl Pts',(44.0191184364596,7.90807633871839,-47.1700481506604));
#21186=CARTESIAN_POINT('Ctrl Pts',(43.9750046174461,7.92280378598205,-47.0072401194241));
#21187=CARTESIAN_POINT('Ctrl Pts',(43.8166697449641,7.7818691906547,-47.947530394193));
#21188=CARTESIAN_POINT('Ctrl Pts',(43.8570720539749,7.77209665345059,-47.8007056846591));
#21189=CARTESIAN_POINT('Ctrl Pts',(43.8766475282555,7.76602646568173,-47.6477355606756));
#21190=CARTESIAN_POINT('Ctrl Pts',(43.8766475282555,7.76602646568173,-47.3522644393244));
#21191=CARTESIAN_POINT('Ctrl Pts',(43.857072053975,7.77209665345058,-47.199294315341));
#21192=CARTESIAN_POINT('Ctrl Pts',(43.8166697449641,7.7818691906547,-47.052469605807));
#21193=CARTESIAN_POINT('Ctrl Pts',(43.658334872482,7.64093459532735,-47.9023009078101));
#21194=CARTESIAN_POINT('Ctrl Pts',(43.6948644867881,7.63597968526781,-47.7714312414787));
#21195=CARTESIAN_POINT('Ctrl Pts',(43.71331135762,7.63258420254192,-47.6333822918808));
#21196=CARTESIAN_POINT('Ctrl Pts',(43.71331135762,7.63258420254192,-47.3666177081192));
#21197=CARTESIAN_POINT('Ctrl Pts',(43.6948644867881,7.63597968526781,-47.2285687585214));
#21198=CARTESIAN_POINT('Ctrl Pts',(43.658334872482,7.64093459532735,-47.0976990921899));
#21199=CARTESIAN_POINT('Ctrl Pts',(43.5,7.5,-47.8570714214271));
#21200=CARTESIAN_POINT('Ctrl Pts',(43.5328181043034,7.5,-47.742185076798));
#21201=CARTESIAN_POINT('Ctrl Pts',(43.5500025534701,7.49916545416939,-47.619029298261));
#21202=CARTESIAN_POINT('Ctrl Pts',(43.5500025534701,7.49916545416939,-47.380970701739));
#21203=CARTESIAN_POINT('Ctrl Pts',(43.5328181043035,7.5,-47.2578149232021));
#21204=CARTESIAN_POINT('Ctrl Pts',(43.5,7.5,-47.1429285785729));
#21205=CARTESIAN_POINT('',(43.5,7.5,-47.1429285785729));
#21206=CARTESIAN_POINT('',(43.5,7.5,-47.1429285785729));
#21207=CARTESIAN_POINT('',(43.5,7.5,-47.8570714214271));
#21208=CARTESIAN_POINT('',(43.9750046174461,7.92280378598205,-47.9927598805759));
#21209=CARTESIAN_POINT('Ctrl Pts',(43.5,7.5,-47.8570714214271));
#21210=CARTESIAN_POINT('Ctrl Pts',(43.5328181043034,7.5,-47.742185076798));
#21211=CARTESIAN_POINT('Ctrl Pts',(43.5500025534701,7.49916545416939,-47.619029298261));
#21212=CARTESIAN_POINT('Ctrl Pts',(43.5500025534701,7.49916545416939,-47.380970701739));
#21213=CARTESIAN_POINT('Ctrl Pts',(43.5328181043035,7.5,-47.2578149232021));
#21214=CARTESIAN_POINT('Ctrl Pts',(43.5,7.5,-47.1429285785729));
#21215=CARTESIAN_POINT('Origin',(42.25,7.75,-47.5));
#21216=CARTESIAN_POINT('',(43.1527777777778,7.5,-46.5645897777175));
#21217=CARTESIAN_POINT('',(43.5,8.,-46.2048166153011));
#21218=CARTESIAN_POINT('',(40.95,7.5,-47.5));
#21219=CARTESIAN_POINT('Origin',(42.25,7.5,-47.5));
#21220=CARTESIAN_POINT('',(43.1527777777778,7.5,-48.4354102222825));
#21221=CARTESIAN_POINT('Origin',(42.25,7.5,-47.5));
#21222=CARTESIAN_POINT('',(43.1527777777778,7.5,-48.4354102222825));
#21223=CARTESIAN_POINT('Ctrl Pts',(43.9750046174461,7.92280378598205,-47.0072401194241));
#21224=CARTESIAN_POINT('Ctrl Pts',(43.8929060558365,7.95021248156921,-46.704244244619));
#21225=CARTESIAN_POINT('Ctrl Pts',(43.7266147755088,8.,-46.4235257747395));
#21226=CARTESIAN_POINT('Ctrl Pts',(43.5,8.,-46.2048166153011));
#21227=CARTESIAN_POINT('Ctrl Pts',(43.8166697449641,7.7818691906547,-47.052469605807));
#21228=CARTESIAN_POINT('Ctrl Pts',(43.7411120931071,7.80014165437948,-46.7775693027908));
#21229=CARTESIAN_POINT('Ctrl Pts',(43.5898911851839,7.83333333333333,-46.5231993141155));
#21230=CARTESIAN_POINT('Ctrl Pts',(43.3842592592593,7.83333333333333,-46.3247410027733));
#21231=CARTESIAN_POINT('Ctrl Pts',(43.658334872482,7.64093459532735,-47.0976990921899));
#21232=CARTESIAN_POINT('Ctrl Pts',(43.5893181303776,7.65007082718974,-46.8508943609626));
#21233=CARTESIAN_POINT('Ctrl Pts',(43.453167594859,7.66666666666667,-46.6228728534914));
#21234=CARTESIAN_POINT('Ctrl Pts',(43.2685185185185,7.66666666666667,-46.4446653902454));
#21235=CARTESIAN_POINT('Ctrl Pts',(43.5,7.5,-47.1429285785729));
#21236=CARTESIAN_POINT('Ctrl Pts',(43.4375241676482,7.5,-46.9242194191345));
#21237=CARTESIAN_POINT('Ctrl Pts',(43.3164440045341,7.5,-46.7225463928674));
#21238=CARTESIAN_POINT('Ctrl Pts',(43.1527777777778,7.5,-46.5645897777175));
#21239=CARTESIAN_POINT('Ctrl Pts',(43.5,7.5,-47.1429285785729));
#21240=CARTESIAN_POINT('Ctrl Pts',(43.4375241676482,7.5,-46.9242194191345));
#21241=CARTESIAN_POINT('Ctrl Pts',(43.3164440045341,7.5,-46.7225463928674));
#21242=CARTESIAN_POINT('Ctrl Pts',(43.1527777777778,7.5,-46.5645897777175));
#21243=CARTESIAN_POINT('Ctrl Pts',(43.5,8.,-48.7951833846989));
#21244=CARTESIAN_POINT('Ctrl Pts',(43.7266147755088,8.,-48.5764742252605));
#21245=CARTESIAN_POINT('Ctrl Pts',(43.8929060558365,7.95021248156921,-48.295755755381));
#21246=CARTESIAN_POINT('Ctrl Pts',(43.9750046174461,7.92280378598205,-47.9927598805759));
#21247=CARTESIAN_POINT('Ctrl Pts',(43.3842592592593,7.83333333333333,-48.6752589972267));
#21248=CARTESIAN_POINT('Ctrl Pts',(43.5898911851839,7.83333333333333,-48.4768006858845));
#21249=CARTESIAN_POINT('Ctrl Pts',(43.7411120931071,7.80014165437948,-48.2224306972092));
#21250=CARTESIAN_POINT('Ctrl Pts',(43.8166697449641,7.7818691906547,-47.947530394193));
#21251=CARTESIAN_POINT('Ctrl Pts',(43.2685185185185,7.66666666666667,-48.5553346097546));
#21252=CARTESIAN_POINT('Ctrl Pts',(43.453167594859,7.66666666666667,-48.3771271465086));
#21253=CARTESIAN_POINT('Ctrl Pts',(43.5893181303776,7.65007082718974,-48.1491056390374));
#21254=CARTESIAN_POINT('Ctrl Pts',(43.658334872482,7.64093459532735,-47.9023009078101));
#21255=CARTESIAN_POINT('Ctrl Pts',(43.1527777777778,7.5,-48.4354102222825));
#21256=CARTESIAN_POINT('Ctrl Pts',(43.3164440045341,7.5,-48.2774536071326));
#21257=CARTESIAN_POINT('Ctrl Pts',(43.4375241676482,7.5,-48.0757805808655));
#21258=CARTESIAN_POINT('Ctrl Pts',(43.5,7.5,-47.8570714214271));
#21259=CARTESIAN_POINT('Ctrl Pts',(43.1527777777778,7.5,-48.4354102222825));
#21260=CARTESIAN_POINT('Ctrl Pts',(43.3164440045341,7.5,-48.2774536071326));
#21261=CARTESIAN_POINT('Ctrl Pts',(43.4375241676482,7.5,-48.0757805808655));
#21262=CARTESIAN_POINT('Ctrl Pts',(43.5,7.5,-47.8570714214271));
#21263=CARTESIAN_POINT('Origin',(42.25,8.,-47.5));
#21264=CARTESIAN_POINT('',(40.95,0.,-47.5));
#21265=CARTESIAN_POINT('',(40.95,8.,-47.5));
#21266=CARTESIAN_POINT('Origin',(42.25,0.,-47.5));
#21267=CARTESIAN_POINT('Ctrl Pts',(-35.9750046174461,7.92280378598206,-47.0072401194241));
#21268=CARTESIAN_POINT('Ctrl Pts',(-36.0191184364596,7.90807633871839,-47.1700481506605));
#21269=CARTESIAN_POINT('Ctrl Pts',(-36.0399563352666,7.8994452073828,-47.337911445339));
#21270=CARTESIAN_POINT('Ctrl Pts',(-36.0399563352666,7.8994452073828,-47.662088554661));
#21271=CARTESIAN_POINT('Ctrl Pts',(-36.0191184364596,7.90807633871838,-47.8299518493395));
#21272=CARTESIAN_POINT('Ctrl Pts',(-35.9750046174461,7.92280378598205,-47.9927598805758));
#21273=CARTESIAN_POINT('Ctrl Pts',(-35.8166697449641,7.78186919065471,-47.0524696058071));
#21274=CARTESIAN_POINT('Ctrl Pts',(-35.857072053975,7.77209665345057,-47.1992943153412));
#21275=CARTESIAN_POINT('Ctrl Pts',(-35.8766475311167,7.76602645901027,-47.3522644389587));
#21276=CARTESIAN_POINT('Ctrl Pts',(-35.8766475311167,7.76602645901027,-47.6477355610413));
#21277=CARTESIAN_POINT('Ctrl Pts',(-35.857072053975,7.77209665345057,-47.8007056846588));
#21278=CARTESIAN_POINT('Ctrl Pts',(-35.8166697449641,7.7818691906547,-47.9475303941929));
#21279=CARTESIAN_POINT('Ctrl Pts',(-35.658334872482,7.64093459532735,-47.09769909219));
#21280=CARTESIAN_POINT('Ctrl Pts',(-35.6948644867881,7.63597968526782,-47.2285687585214));
#21281=CARTESIAN_POINT('Ctrl Pts',(-35.7133113651929,7.63258419989791,-47.3666177074644));
#21282=CARTESIAN_POINT('Ctrl Pts',(-35.7133113651929,7.63258419989791,-47.6333822925356));
#21283=CARTESIAN_POINT('Ctrl Pts',(-35.6948644867881,7.63597968526782,-47.7714312414786));
#21284=CARTESIAN_POINT('Ctrl Pts',(-35.6583348724821,7.64093459532735,-47.90230090781));
#21285=CARTESIAN_POINT('Ctrl Pts',(-35.5,7.5,-47.1429285785729));
#21286=CARTESIAN_POINT('Ctrl Pts',(-35.5328181043034,7.5,-47.2578149232021));
#21287=CARTESIAN_POINT('Ctrl Pts',(-35.550002561043,7.49916545152538,-47.3809707010842));
#21288=CARTESIAN_POINT('Ctrl Pts',(-35.550002561043,7.49916545152537,-47.6190292989158));
#21289=CARTESIAN_POINT('Ctrl Pts',(-35.5328181043034,7.5,-47.7421850767979));
#21290=CARTESIAN_POINT('Ctrl Pts',(-35.5,7.5,-47.8570714214271));
#21291=CARTESIAN_POINT('',(-35.5,7.5,-47.8570714214271));
#21292=CARTESIAN_POINT('',(-35.5,7.5,-47.8570714214271));
#21293=CARTESIAN_POINT('',(-35.5,7.5,-47.1429285785729));
#21294=CARTESIAN_POINT('',(-35.9750046174461,7.92280378598206,-47.0072401194241));
#21295=CARTESIAN_POINT('',(-35.550002561043,7.49916545152538,-47.5));
#21296=CARTESIAN_POINT('Ctrl Pts',(-35.5,7.5,-47.1429285785729));
#21297=CARTESIAN_POINT('Ctrl Pts',(-35.5328181043034,7.5,-47.2578149232021));
#21298=CARTESIAN_POINT('Ctrl Pts',(-35.550002561043,7.49916545152538,-47.3809707010842));
#21299=CARTESIAN_POINT('Ctrl Pts',(-35.550002561043,7.49916545152538,-47.5));
#21300=CARTESIAN_POINT('Ctrl Pts',(-35.550002561043,7.49916545152538,-47.5));
#21301=CARTESIAN_POINT('Ctrl Pts',(-35.550002561043,7.49916545152537,-47.6190292989158));
#21302=CARTESIAN_POINT('Ctrl Pts',(-35.5328181043034,7.5,-47.7421850767979));
#21303=CARTESIAN_POINT('Ctrl Pts',(-35.5,7.5,-47.8570714214271));
#21304=CARTESIAN_POINT('Origin',(-34.25,7.75,-47.5));
#21305=CARTESIAN_POINT('',(-35.1527777777778,7.5,-48.4354102222825));
#21306=CARTESIAN_POINT('',(-35.5,8.,-48.7951833846989));
#21307=CARTESIAN_POINT('',(-35.1527777777778,7.5,-46.5645897777175));
#21308=CARTESIAN_POINT('Origin',(-34.25,7.5,-47.5));
#21309=CARTESIAN_POINT('',(-35.1527777777778,7.5,-46.5645897777175));
#21310=CARTESIAN_POINT('Ctrl Pts',(-35.9750046174461,7.92280378598205,-47.9927598805758));
#21311=CARTESIAN_POINT('Ctrl Pts',(-35.8929060558365,7.95021248156921,-48.295755755381));
#21312=CARTESIAN_POINT('Ctrl Pts',(-35.7266147755088,8.,-48.5764742252605));
#21313=CARTESIAN_POINT('Ctrl Pts',(-35.5,8.,-48.7951833846989));
#21314=CARTESIAN_POINT('Ctrl Pts',(-35.8166697449641,7.7818691906547,-47.9475303941929));
#21315=CARTESIAN_POINT('Ctrl Pts',(-35.7411120931071,7.80014165437948,-48.2224306972092));
#21316=CARTESIAN_POINT('Ctrl Pts',(-35.5898911851839,7.83333333333334,-48.4768006858845));
#21317=CARTESIAN_POINT('Ctrl Pts',(-35.3842592592593,7.83333333333333,-48.6752589972267));
#21318=CARTESIAN_POINT('Ctrl Pts',(-35.6583348724821,7.64093459532735,-47.90230090781));
#21319=CARTESIAN_POINT('Ctrl Pts',(-35.5893181303776,7.65007082718974,-48.1491056390373));
#21320=CARTESIAN_POINT('Ctrl Pts',(-35.453167594859,7.66666666666667,-48.3771271465086));
#21321=CARTESIAN_POINT('Ctrl Pts',(-35.2685185185185,7.66666666666667,-48.5553346097546));
#21322=CARTESIAN_POINT('Ctrl Pts',(-35.5,7.5,-47.8570714214271));
#21323=CARTESIAN_POINT('Ctrl Pts',(-35.4375241676482,7.5,-48.0757805808655));
#21324=CARTESIAN_POINT('Ctrl Pts',(-35.3164440045342,7.5,-48.2774536071326));
#21325=CARTESIAN_POINT('Ctrl Pts',(-35.1527777777778,7.5,-48.4354102222825));
#21326=CARTESIAN_POINT('Ctrl Pts',(-35.5,7.5,-47.8570714214271));
#21327=CARTESIAN_POINT('Ctrl Pts',(-35.4375241676482,7.5,-48.0757805808655));
#21328=CARTESIAN_POINT('Ctrl Pts',(-35.3164440045342,7.5,-48.2774536071326));
#21329=CARTESIAN_POINT('Ctrl Pts',(-35.1527777777778,7.5,-48.4354102222825));
#21330=CARTESIAN_POINT('Ctrl Pts',(-35.5,8.,-46.2048166153011));
#21331=CARTESIAN_POINT('Ctrl Pts',(-35.7266147755088,8.,-46.4235257747395));
#21332=CARTESIAN_POINT('Ctrl Pts',(-35.8929060558365,7.95021248156921,-46.704244244619));
#21333=CARTESIAN_POINT('Ctrl Pts',(-35.9750046174461,7.92280378598206,-47.0072401194241));
#21334=CARTESIAN_POINT('Ctrl Pts',(-35.3842592592593,7.83333333333333,-46.3247410027733));
#21335=CARTESIAN_POINT('Ctrl Pts',(-35.5898911851839,7.83333333333333,-46.5231993141155));
#21336=CARTESIAN_POINT('Ctrl Pts',(-35.7411120931071,7.80014165437948,-46.7775693027908));
#21337=CARTESIAN_POINT('Ctrl Pts',(-35.8166697449641,7.7818691906547,-47.0524696058071));
#21338=CARTESIAN_POINT('Ctrl Pts',(-35.2685185185185,7.66666666666667,-46.4446653902454));
#21339=CARTESIAN_POINT('Ctrl Pts',(-35.4531675948591,7.66666666666667,-46.6228728534915));
#21340=CARTESIAN_POINT('Ctrl Pts',(-35.5893181303776,7.65007082718974,-46.8508943609627));
#21341=CARTESIAN_POINT('Ctrl Pts',(-35.658334872482,7.64093459532735,-47.09769909219));
#21342=CARTESIAN_POINT('Ctrl Pts',(-35.1527777777778,7.5,-46.5645897777175));
#21343=CARTESIAN_POINT('Ctrl Pts',(-35.3164440045342,7.5,-46.7225463928674));
#21344=CARTESIAN_POINT('Ctrl Pts',(-35.4375241676482,7.5,-46.9242194191345));
#21345=CARTESIAN_POINT('Ctrl Pts',(-35.5,7.5,-47.1429285785729));
#21346=CARTESIAN_POINT('Ctrl Pts',(-35.1527777777778,7.5,-46.5645897777175));
#21347=CARTESIAN_POINT('Ctrl Pts',(-35.3164440045342,7.5,-46.7225463928674));
#21348=CARTESIAN_POINT('Ctrl Pts',(-35.4375241676482,7.5,-46.9242194191345));
#21349=CARTESIAN_POINT('Ctrl Pts',(-35.5,7.5,-47.1429285785729));
#21350=CARTESIAN_POINT('Origin',(-34.25,8.,-47.5));
#21351=CARTESIAN_POINT('',(-35.55,0.,-47.5));
#21352=CARTESIAN_POINT('',(-35.55,8.,-47.5));
#21353=CARTESIAN_POINT('Origin',(-34.25,0.,-47.5));
#21354=CARTESIAN_POINT('Origin',(44.75,-3.,-47.5));
#21355=CARTESIAN_POINT('',(44.5,-3.,-45.));
#21356=CARTESIAN_POINT('',(44.75,-3.,-44.75));
#21357=CARTESIAN_POINT('Origin',(44.5,-3.,-47.5));
#21358=CARTESIAN_POINT('Origin',(45.,-3.,-47.5));
#21359=CARTESIAN_POINT('',(40.,-3.,-45.));
#21360=CARTESIAN_POINT('',(45.,-3.,-45.));
#21361=CARTESIAN_POINT('Origin',(40.,-3.,-47.5));
#21362=CARTESIAN_POINT('Origin',(39.75,-3.,-47.5));
#21363=CARTESIAN_POINT('',(39.5,-3.,-44.5));
#21364=CARTESIAN_POINT('Origin',(39.5,-3.,-47.5));
#21365=CARTESIAN_POINT('',(39.75,-3.,-44.75));
#21366=CARTESIAN_POINT('Origin',(39.5,8.,-53.));
#21367=CARTESIAN_POINT('',(39.5,-9.,-42.));
#21368=CARTESIAN_POINT('',(39.5,-9.,-53.));
#21369=CARTESIAN_POINT('',(39.5,8.,-42.));
#21370=CARTESIAN_POINT('Origin',(-34.25,0.,-47.5));
#21371=CARTESIAN_POINT('Origin',(42.25,0.,-47.5));
#21372=CARTESIAN_POINT('Origin',(-25.2,-3.55,-30.9504065443768));
#21373=CARTESIAN_POINT('',(-25.2,-3.55,-30.9504065443768));
#21374=CARTESIAN_POINT('Origin',(-25.2,-3.55,-35.0495934556232));
#21375=CARTESIAN_POINT('',(-25.2,-3.55,-35.0495934556232));
#21376=CARTESIAN_POINT('Origin',(-25.2,-5.55111512312578E-16,-37.0991869112463));
#21377=CARTESIAN_POINT('Origin',(25.2,-3.55,-35.0495934556232));
#21378=CARTESIAN_POINT('',(25.2,-3.55,-35.0495934556232));
#21379=CARTESIAN_POINT('Origin',(25.2,-3.55,-30.9504065443768));
#21380=CARTESIAN_POINT('',(25.2,-3.55,-30.9504065443768));
#21381=CARTESIAN_POINT('Origin',(25.2,2.51002806498228E-16,-28.9008130887537));
#21382=CARTESIAN_POINT('Origin',(39.5,8.,-42.));
#21383=CARTESIAN_POINT('',(39.5,-9.,-42.));
#21384=CARTESIAN_POINT('Origin',(4.,-9.,-47.5));
#21385=CARTESIAN_POINT('Origin',(18.,5.,-37.5));
#21386=CARTESIAN_POINT('',(0.,0.,0.));
#21387=CARTESIAN_POINT('Origin',(24.,8.1,-47.5));
#21388=CARTESIAN_POINT('',(19.6,8.,-47.5));
#21389=CARTESIAN_POINT('Origin',(24.,8.,-47.5));
#21390=CARTESIAN_POINT('',(19.8,8.2,-47.5));
#21391=CARTESIAN_POINT('',(19.7,8.1,-47.5));
#21392=CARTESIAN_POINT('Origin',(24.,8.2,-47.5));
#21393=CARTESIAN_POINT('Origin',(24.,11.,-47.5));
#21394=CARTESIAN_POINT('',(19.8,10.8,-47.5));
#21395=CARTESIAN_POINT('Origin',(24.,10.8,-47.5));
#21396=CARTESIAN_POINT('',(19.8,11.,-47.5));
#21397=CARTESIAN_POINT('Origin',(3.99999999999999,8.,-47.5));
#21398=CARTESIAN_POINT('',(43.5,8.,-54.8));
#21399=CARTESIAN_POINT('',(-35.5,8.,-54.8));
#21400=CARTESIAN_POINT('',(24.5,8.,-54.8));
#21401=CARTESIAN_POINT('',(44.8,8.,-53.5));
#21402=CARTESIAN_POINT('Origin',(43.5,8.,-53.5));
#21403=CARTESIAN_POINT('',(44.8,8.,-41.5));
#21404=CARTESIAN_POINT('',(44.8,8.,-43.75));
#21405=CARTESIAN_POINT('',(43.5,8.,-40.2));
#21406=CARTESIAN_POINT('Origin',(43.5,8.,-41.5));
#21407=CARTESIAN_POINT('',(-35.5,8.,-40.2));
#21408=CARTESIAN_POINT('',(-16.5,8.,-40.2));
#21409=CARTESIAN_POINT('',(-36.8,8.,-41.5));
#21410=CARTESIAN_POINT('Origin',(-35.5,8.,-41.5));
#21411=CARTESIAN_POINT('',(-36.8,8.,-53.5));
#21412=CARTESIAN_POINT('',(-36.8,8.,-51.25));
#21413=CARTESIAN_POINT('Origin',(-35.5,8.,-53.5));
#21414=CARTESIAN_POINT('',(-35.7,8.,-47.5));
#21415=CARTESIAN_POINT('Origin',(-34.25,8.,-47.5));
#21416=CARTESIAN_POINT('',(40.8,8.,-47.5));
#21417=CARTESIAN_POINT('Origin',(42.25,8.,-47.5));
#21418=CARTESIAN_POINT('Origin',(24.,10.9,-47.5));
#21419=CARTESIAN_POINT('',(19.6,11.,-47.5));
#21420=CARTESIAN_POINT('Origin',(24.,11.,-47.5));
#21421=CARTESIAN_POINT('',(19.7,10.9,-47.5));
#21422=CARTESIAN_POINT('Origin',(3.99999999999999,11.,-47.5));
#21423=CARTESIAN_POINT('',(43.5,11.,-40.7));
#21424=CARTESIAN_POINT('',(-35.5,11.,-40.7));
#21425=CARTESIAN_POINT('',(-6.25,11.,-40.7));
#21426=CARTESIAN_POINT('',(44.3,11.,-41.5));
#21427=CARTESIAN_POINT('Origin',(43.5,11.,-41.5));
#21428=CARTESIAN_POINT('',(44.3,11.,-53.5));
#21429=CARTESIAN_POINT('',(44.3,11.,-45.625));
#21430=CARTESIAN_POINT('',(43.5,11.,-54.3));
#21431=CARTESIAN_POINT('Origin',(43.5,11.,-53.5));
#21432=CARTESIAN_POINT('',(-35.5,11.,-54.3));
#21433=CARTESIAN_POINT('',(14.25,11.,-54.3));
#21434=CARTESIAN_POINT('',(-36.3,11.,-53.5));
#21435=CARTESIAN_POINT('Origin',(-35.5,11.,-53.5));
#21436=CARTESIAN_POINT('',(-36.3,11.,-41.5));
#21437=CARTESIAN_POINT('',(-36.3,11.,-49.375));
#21438=CARTESIAN_POINT('Origin',(-35.5,11.,-41.5));
#21439=CARTESIAN_POINT('',(40.8,11.,-47.5));
#21440=CARTESIAN_POINT('Origin',(42.25,11.,-47.5));
#21441=CARTESIAN_POINT('',(-35.7,11.,-47.5));
#21442=CARTESIAN_POINT('Origin',(-34.25,11.,-47.5));
#21443=CARTESIAN_POINT('Origin',(24.5,8.1,-54.9));
#21444=CARTESIAN_POINT('',(43.5,8.2,-55.));
#21445=CARTESIAN_POINT('',(43.5,8.2,-55.));
#21446=CARTESIAN_POINT('',(-35.5,8.2,-55.));
#21447=CARTESIAN_POINT('',(-35.5,8.,-54.8));
#21448=CARTESIAN_POINT('',(24.5,8.2,-55.));
#21449=CARTESIAN_POINT('Origin',(43.5,8.1,-53.5));
#21450=CARTESIAN_POINT('',(45.,8.2,-53.5));
#21451=CARTESIAN_POINT('Origin',(43.5,8.2,-53.5));
#21452=CARTESIAN_POINT('',(45.,8.2,-53.5));
#21453=CARTESIAN_POINT('Origin',(44.9,8.1,-43.75));
#21454=CARTESIAN_POINT('',(45.,8.2,-41.5));
#21455=CARTESIAN_POINT('',(45.,8.2,-41.5));
#21456=CARTESIAN_POINT('',(45.,8.2,-43.75));
#21457=CARTESIAN_POINT('Origin',(43.5,8.1,-41.5));
#21458=CARTESIAN_POINT('',(43.5,8.2,-40.));
#21459=CARTESIAN_POINT('Origin',(43.5,8.2,-41.5));
#21460=CARTESIAN_POINT('',(43.5,8.2,-40.));
#21461=CARTESIAN_POINT('Origin',(-16.5,8.1,-40.1));
#21462=CARTESIAN_POINT('',(-35.5,8.2,-40.));
#21463=CARTESIAN_POINT('',(-35.5,8.2,-40.));
#21464=CARTESIAN_POINT('',(-16.5,8.2,-40.));
#21465=CARTESIAN_POINT('Origin',(-35.5,8.1,-41.5));
#21466=CARTESIAN_POINT('',(-37.,8.2,-41.5));
#21467=CARTESIAN_POINT('Origin',(-35.5,8.2,-41.5));
#21468=CARTESIAN_POINT('',(-37.,8.2,-41.5));
#21469=CARTESIAN_POINT('Origin',(-36.9,8.1,-51.25));
#21470=CARTESIAN_POINT('',(-37.,8.2,-53.5));
#21471=CARTESIAN_POINT('',(-37.,8.2,-53.5));
#21472=CARTESIAN_POINT('',(-37.,8.2,-51.25));
#21473=CARTESIAN_POINT('Origin',(-35.5,8.1,-53.5));
#21474=CARTESIAN_POINT('Origin',(-35.5,8.2,-53.5));
#21475=CARTESIAN_POINT('Origin',(43.5,8.,-41.5));
#21476=CARTESIAN_POINT('',(45.,10.3,-41.5));
#21477=CARTESIAN_POINT('',(45.,8.,-41.5));
#21478=CARTESIAN_POINT('',(43.5,10.3,-40.));
#21479=CARTESIAN_POINT('Origin',(43.5,10.3,-41.5));
#21480=CARTESIAN_POINT('',(43.5,8.,-40.));
#21481=CARTESIAN_POINT('Origin',(45.,8.,-40.));
#21482=CARTESIAN_POINT('',(45.,10.3,-53.5));
#21483=CARTESIAN_POINT('',(45.,8.,-53.5));
#21484=CARTESIAN_POINT('',(45.,10.3,-41.875));
#21485=CARTESIAN_POINT('Origin',(43.5,8.,-53.5));
#21486=CARTESIAN_POINT('',(43.5,10.3,-55.));
#21487=CARTESIAN_POINT('',(43.5,8.,-55.));
#21488=CARTESIAN_POINT('Origin',(43.5,10.3,-53.5));
#21489=CARTESIAN_POINT('Origin',(45.,8.,-55.));
#21490=CARTESIAN_POINT('',(-35.5,10.3,-55.));
#21491=CARTESIAN_POINT('',(-35.5,8.,-55.));
#21492=CARTESIAN_POINT('',(34.75,10.3,-55.));
#21493=CARTESIAN_POINT('Origin',(-26.75,10.4707106781187,-40.0707106781187));
#21494=CARTESIAN_POINT('',(43.5,10.6414213562373,-40.1414213562373));
#21495=CARTESIAN_POINT('',(43.5,10.3,-40.));
#21496=CARTESIAN_POINT('',(-35.5,10.6414213562373,-40.1414213562373));
#21497=CARTESIAN_POINT('',(-26.75,10.6414213562373,-40.1414213562373));
#21498=CARTESIAN_POINT('',(-35.5,10.3,-40.));
#21499=CARTESIAN_POINT('',(-35.5,10.6414213562373,-40.1414213562373));
#21500=CARTESIAN_POINT('',(-26.75,10.3,-40.));
#21501=CARTESIAN_POINT('Origin',(43.5,10.4707106781187,-41.5));
#21502=CARTESIAN_POINT('',(44.8585786437627,10.6414213562373,-41.5));
#21503=CARTESIAN_POINT('',(45.,10.3,-41.5));
#21504=CARTESIAN_POINT('Origin',(43.5,10.6414213562373,-41.5));
#21505=CARTESIAN_POINT('Origin',(44.9292893218813,10.4707106781187,-41.875));
#21506=CARTESIAN_POINT('',(44.8585786437627,10.6414213562373,-53.5));
#21507=CARTESIAN_POINT('',(45.,10.3,-53.5));
#21508=CARTESIAN_POINT('',(44.8585786437627,10.6414213562373,-41.875));
#21509=CARTESIAN_POINT('Origin',(43.5,10.4707106781187,-53.5));
#21510=CARTESIAN_POINT('',(43.5,10.6414213562373,-54.8585786437627));
#21511=CARTESIAN_POINT('',(43.5,10.3,-55.));
#21512=CARTESIAN_POINT('Origin',(43.5,10.6414213562373,-53.5));
#21513=CARTESIAN_POINT('Origin',(34.75,10.4707106781187,-54.9292893218813));
#21514=CARTESIAN_POINT('',(-35.5,10.6414213562373,-54.8585786437627));
#21515=CARTESIAN_POINT('',(-35.5,10.3,-55.));
#21516=CARTESIAN_POINT('',(34.75,10.6414213562373,-54.8585786437627));
#21517=CARTESIAN_POINT('Origin',(-35.5,10.4707106781187,-53.5));
#21518=CARTESIAN_POINT('',(-37.,10.3,-53.5));
#21519=CARTESIAN_POINT('',(-36.8585786437627,10.6414213562373,-53.5));
#21520=CARTESIAN_POINT('',(-37.,10.3,-53.5));
#21521=CARTESIAN_POINT('Origin',(-35.5,10.6414213562373,-53.5));
#21522=CARTESIAN_POINT('Origin',(-35.5,10.3,-53.5));
#21523=CARTESIAN_POINT('Origin',(-36.9292893218813,10.4707106781187,-53.125));
#21524=CARTESIAN_POINT('',(-37.,10.3,-41.5));
#21525=CARTESIAN_POINT('',(-36.8585786437627,10.6414213562373,-41.5));
#21526=CARTESIAN_POINT('',(-37.,10.3,-41.5));
#21527=CARTESIAN_POINT('',(-36.8585786437627,10.6414213562373,-53.125));
#21528=CARTESIAN_POINT('',(-37.,10.3,-53.125));
#21529=CARTESIAN_POINT('Origin',(-35.5,10.4707106781187,-41.5));
#21530=CARTESIAN_POINT('Origin',(-35.5,10.6414213562373,-41.5));
#21531=CARTESIAN_POINT('Origin',(-35.5,10.3,-41.5));
#21532=CARTESIAN_POINT('Origin',(-35.5,10.75,-53.5));
#21533=CARTESIAN_POINT('',(-36.6414213562373,10.8585786437627,-53.5));
#21534=CARTESIAN_POINT('',(-36.5,11.,-53.5));
#21535=CARTESIAN_POINT('',(-35.5,10.8585786437627,-54.6414213562373));
#21536=CARTESIAN_POINT('Origin',(-35.5,10.8585786437627,-53.5));
#21537=CARTESIAN_POINT('',(-35.5,11.,-54.5));
#21538=CARTESIAN_POINT('Origin',(-36.75,10.75,-51.25));
#21539=CARTESIAN_POINT('',(-36.6414213562373,10.8585786437627,-41.5));
#21540=CARTESIAN_POINT('',(-36.5,11.,-41.5));
#21541=CARTESIAN_POINT('',(-36.6414213562373,10.8585786437627,-49.375));
#21542=CARTESIAN_POINT('Origin',(-35.5,10.75,-41.5));
#21543=CARTESIAN_POINT('',(-35.5,10.8585786437627,-40.3585786437627));
#21544=CARTESIAN_POINT('',(-35.5,11.,-40.5));
#21545=CARTESIAN_POINT('Origin',(-35.5,10.8585786437627,-41.5));
#21546=CARTESIAN_POINT('Origin',(-16.5,10.75,-40.25));
#21547=CARTESIAN_POINT('',(43.5,10.8585786437627,-40.3585786437627));
#21548=CARTESIAN_POINT('',(43.5,11.,-40.5));
#21549=CARTESIAN_POINT('',(-6.25,10.8585786437627,-40.3585786437627));
#21550=CARTESIAN_POINT('Origin',(-37.,8.,-40.));
#21551=CARTESIAN_POINT('',(-35.5,8.,-40.));
#21552=CARTESIAN_POINT('Origin',(-6.25,10.9292893218813,-40.5292893218813));
#21553=CARTESIAN_POINT('',(-35.5,11.,-40.7));
#21554=CARTESIAN_POINT('',(43.5,10.8585786437627,-40.3585786437627));
#21555=CARTESIAN_POINT('Origin',(-35.5,10.9292893218813,-41.5));
#21556=CARTESIAN_POINT('',(-36.3,11.,-41.5));
#21557=CARTESIAN_POINT('Origin',(-36.4707106781187,10.9292893218813,-49.375));
#21558=CARTESIAN_POINT('',(-36.3,11.,-53.5));
#21559=CARTESIAN_POINT('Origin',(-35.5,10.9292893218813,-53.5));
#21560=CARTESIAN_POINT('',(-35.5,11.,-54.3));
#21561=CARTESIAN_POINT('Origin',(14.25,10.9292893218813,-54.4707106781187));
#21562=CARTESIAN_POINT('',(43.5,10.8585786437627,-54.6414213562373));
#21563=CARTESIAN_POINT('',(43.5,11.,-54.3));
#21564=CARTESIAN_POINT('',(14.25,10.8585786437627,-54.6414213562373));
#21565=CARTESIAN_POINT('Origin',(43.5,10.9292893218813,-53.5));
#21566=CARTESIAN_POINT('',(44.6414213562373,10.8585786437627,-53.5));
#21567=CARTESIAN_POINT('',(44.3,11.,-53.5));
#21568=CARTESIAN_POINT('Origin',(43.5,10.8585786437627,-53.5));
#21569=CARTESIAN_POINT('Origin',(44.4707106781187,10.9292893218813,-45.625));
#21570=CARTESIAN_POINT('',(44.6414213562373,10.8585786437627,-41.5));
#21571=CARTESIAN_POINT('',(44.3,11.,-41.5));
#21572=CARTESIAN_POINT('',(44.6414213562373,10.8585786437627,-45.625));
#21573=CARTESIAN_POINT('Origin',(43.5,10.9292893218813,-41.5));
#21574=CARTESIAN_POINT('Origin',(43.5,10.8585786437627,-41.5));
#21575=CARTESIAN_POINT('Origin',(43.5,10.75,-53.5));
#21576=CARTESIAN_POINT('',(43.5,11.,-54.5));
#21577=CARTESIAN_POINT('',(44.5,11.,-53.5));
#21578=CARTESIAN_POINT('Origin',(44.75,10.75,-43.75));
#21579=CARTESIAN_POINT('',(45.,10.5,-41.5));
#21580=CARTESIAN_POINT('Origin',(43.5,10.75,-41.5));
#21581=CARTESIAN_POINT('Origin',(24.5,10.75,-54.75));
#21582=CARTESIAN_POINT('Origin',(-34.25,11.,-47.5));
#21583=CARTESIAN_POINT('',(-35.7,11.,-47.5));
#21584=CARTESIAN_POINT('Origin',(42.25,11.,-47.5));
#21585=CARTESIAN_POINT('',(40.8,11.,-47.5));
#21586=CARTESIAN_POINT('Origin',(-35.5,8.,-53.5));
#21587=CARTESIAN_POINT('',(-37.,8.,-53.5));
#21588=CARTESIAN_POINT('Origin',(-35.5,8.,-41.5));
#21589=CARTESIAN_POINT('',(-37.,8.,-41.5));
#21590=CARTESIAN_POINT('Origin',(-37.,8.,-55.));
#21591=CARTESIAN_POINT('',(0.,0.,0.));
#21592=CARTESIAN_POINT('Origin',(-22.,-7.8,-50.));
#21593=CARTESIAN_POINT('',(-22.,-7.8,-45.));
#21594=CARTESIAN_POINT('',(-22.,-7.8,-50.));
#21595=CARTESIAN_POINT('',(-22.,-7.8,-48.75));
#21596=CARTESIAN_POINT('',(-22.,-6.6,-45.));
#21597=CARTESIAN_POINT('',(-22.,-7.8,-45.));
#21598=CARTESIAN_POINT('',(-22.,-6.6,-50.));
#21599=CARTESIAN_POINT('',(-22.,-6.6,-45.));
#21600=CARTESIAN_POINT('',(-22.,-7.8,-50.));
#21601=CARTESIAN_POINT('Origin',(-14.,-7.8,-50.));
#21602=CARTESIAN_POINT('',(-14.,-7.8,-50.));
#21603=CARTESIAN_POINT('',(-5.,-7.8,-50.));
#21604=CARTESIAN_POINT('',(-14.,-6.6,-50.));
#21605=CARTESIAN_POINT('',(-22.,-6.6,-50.));
#21606=CARTESIAN_POINT('',(-14.,-7.8,-50.));
#21607=CARTESIAN_POINT('Origin',(-14.,-7.8,-45.));
#21608=CARTESIAN_POINT('',(-14.,-7.8,-45.));
#21609=CARTESIAN_POINT('',(-14.,-7.8,-46.25));
#21610=CARTESIAN_POINT('',(-14.,-6.6,-45.));
#21611=CARTESIAN_POINT('',(-14.,-6.6,-50.));
#21612=CARTESIAN_POINT('',(-14.,-7.8,-45.));
#21613=CARTESIAN_POINT('Origin',(-22.,-7.8,-45.));
#21614=CARTESIAN_POINT('',(-9.,-7.8,-45.));
#21615=CARTESIAN_POINT('',(-14.,-6.6,-45.));
#21616=CARTESIAN_POINT('Origin',(-18.,-6.6,-47.5));
#21617=CARTESIAN_POINT('Origin',(-6.,-7.8,-51.));
#21618=CARTESIAN_POINT('',(-6.,-7.8,-44.));
#21619=CARTESIAN_POINT('',(-6.,-7.8,-51.));
#21620=CARTESIAN_POINT('',(-6.,-7.8,-49.25));
#21621=CARTESIAN_POINT('',(-6.,-6.8,-44.));
#21622=CARTESIAN_POINT('',(-6.,-7.8,-44.));
#21623=CARTESIAN_POINT('',(-6.,-6.8,-51.));
#21624=CARTESIAN_POINT('',(-6.,-6.8,-44.));
#21625=CARTESIAN_POINT('',(-6.,-7.8,-51.));
#21626=CARTESIAN_POINT('Origin',(2.,-7.8,-51.));
#21627=CARTESIAN_POINT('',(2.,-7.8,-51.));
#21628=CARTESIAN_POINT('',(3.,-7.8,-51.));
#21629=CARTESIAN_POINT('',(2.,-6.8,-51.));
#21630=CARTESIAN_POINT('',(-6.,-6.8,-51.));
#21631=CARTESIAN_POINT('',(2.,-7.8,-51.));
#21632=CARTESIAN_POINT('Origin',(2.,-7.8,-44.));
#21633=CARTESIAN_POINT('',(2.,-7.8,-44.));
#21634=CARTESIAN_POINT('',(2.,-7.8,-45.75));
#21635=CARTESIAN_POINT('',(2.,-6.8,-44.));
#21636=CARTESIAN_POINT('',(2.,-6.8,-51.));
#21637=CARTESIAN_POINT('',(2.,-7.8,-44.));
#21638=CARTESIAN_POINT('Origin',(-6.,-7.8,-44.));
#21639=CARTESIAN_POINT('',(-1.,-7.8,-44.));
#21640=CARTESIAN_POINT('',(2.,-6.8,-44.));
#21641=CARTESIAN_POINT('Origin',(-2.,-6.8,-47.5));
#21642=CARTESIAN_POINT('Origin',(33.,-7.8,-50.));
#21643=CARTESIAN_POINT('',(33.,-7.8,-45.));
#21644=CARTESIAN_POINT('',(33.,-7.8,-50.));
#21645=CARTESIAN_POINT('',(33.,-7.8,-48.75));
#21646=CARTESIAN_POINT('',(33.,-5.4,-45.));
#21647=CARTESIAN_POINT('',(33.,-7.8,-45.));
#21648=CARTESIAN_POINT('',(33.,-5.4,-50.));
#21649=CARTESIAN_POINT('',(33.,-5.4,-45.));
#21650=CARTESIAN_POINT('',(33.,-7.8,-50.));
#21651=CARTESIAN_POINT('Origin',(38.5,-7.8,-50.));
#21652=CARTESIAN_POINT('',(38.5,-7.8,-50.));
#21653=CARTESIAN_POINT('',(21.25,-7.8,-50.));
#21654=CARTESIAN_POINT('',(38.5,-5.4,-50.));
#21655=CARTESIAN_POINT('',(33.,-5.4,-50.));
#21656=CARTESIAN_POINT('',(38.5,-7.8,-50.));
#21657=CARTESIAN_POINT('Origin',(38.5,-7.8,-45.));
#21658=CARTESIAN_POINT('',(38.5,-7.8,-45.));
#21659=CARTESIAN_POINT('',(38.5,-7.8,-46.25));
#21660=CARTESIAN_POINT('',(38.5,-5.4,-45.));
#21661=CARTESIAN_POINT('',(38.5,-5.4,-50.));
#21662=CARTESIAN_POINT('',(38.5,-7.8,-45.));
#21663=CARTESIAN_POINT('Origin',(33.,-7.8,-45.));
#21664=CARTESIAN_POINT('',(18.5,-7.8,-45.));
#21665=CARTESIAN_POINT('',(38.5,-5.4,-45.));
#21666=CARTESIAN_POINT('Origin',(35.75,-5.4,-47.5));
#21667=CARTESIAN_POINT('Origin',(-31.,-9.,-52.8));
#21668=CARTESIAN_POINT('',(-31.,-9.,-42.2));
#21669=CARTESIAN_POINT('',(-31.,-9.,-52.8));
#21670=CARTESIAN_POINT('',(-31.,-9.,-42.2));
#21671=CARTESIAN_POINT('',(-31.,-7.8,-42.2));
#21672=CARTESIAN_POINT('',(-31.,-9.,-42.2));
#21673=CARTESIAN_POINT('',(-31.,-7.8,-52.8));
#21674=CARTESIAN_POINT('',(-31.,-7.8,-42.2));
#21675=CARTESIAN_POINT('',(-31.,-9.,-52.8));
#21676=CARTESIAN_POINT('Origin',(39.,-9.,-52.8));
#21677=CARTESIAN_POINT('',(39.,-9.,-52.8));
#21678=CARTESIAN_POINT('',(-31.,-9.,-52.8));
#21679=CARTESIAN_POINT('',(39.,-7.8,-52.8));
#21680=CARTESIAN_POINT('',(-31.,-7.8,-52.8));
#21681=CARTESIAN_POINT('',(39.,-9.,-52.8));
#21682=CARTESIAN_POINT('Origin',(39.,-9.,-42.2));
#21683=CARTESIAN_POINT('',(39.,-9.,-42.2));
#21684=CARTESIAN_POINT('',(39.,-9.,-52.8));
#21685=CARTESIAN_POINT('',(39.,-7.8,-42.2));
#21686=CARTESIAN_POINT('',(39.,-7.8,-52.8));
#21687=CARTESIAN_POINT('',(39.,-9.,-42.2));
#21688=CARTESIAN_POINT('Origin',(-31.,-9.,-42.2));
#21689=CARTESIAN_POINT('',(39.,-9.,-42.2));
#21690=CARTESIAN_POINT('',(39.,-7.8,-42.2));
#21691=CARTESIAN_POINT('Origin',(4.,-7.8,-47.5));
#21692=CARTESIAN_POINT('Origin',(4.,-9.,-47.5));
#21693=CARTESIAN_POINT('',(0.,0.,0.));
#21694=CARTESIAN_POINT('Origin',(28.61,1.61,-52.5));
#21695=CARTESIAN_POINT('',(29.,1.61,-52.11));
#21696=CARTESIAN_POINT('',(28.61,2.,-52.11));
#21697=CARTESIAN_POINT('',(29.,1.61,-52.11));
#21698=CARTESIAN_POINT('',(28.61,1.61,-52.5));
#21699=CARTESIAN_POINT('',(28.61,1.61,-52.5));
#21700=CARTESIAN_POINT('',(28.61,2.,-52.11));
#21701=CARTESIAN_POINT('Origin',(29.,1.61,-42.89));
#21702=CARTESIAN_POINT('',(28.61,1.61,-42.5));
#21703=CARTESIAN_POINT('',(28.61,2.,-42.89));
#21704=CARTESIAN_POINT('',(28.61,1.61,-42.5));
#21705=CARTESIAN_POINT('',(29.,1.61,-42.89));
#21706=CARTESIAN_POINT('',(29.,1.61,-42.89));
#21707=CARTESIAN_POINT('',(28.61,2.,-42.89));
#21708=CARTESIAN_POINT('Origin',(28.61,-7.8,-52.11));
#21709=CARTESIAN_POINT('',(29.,-7.41,-52.11));
#21710=CARTESIAN_POINT('',(28.61,-7.41,-52.5));
#21711=CARTESIAN_POINT('',(29.,-7.41,-52.11));
#21712=CARTESIAN_POINT('',(28.61,-7.8,-52.11));
#21713=CARTESIAN_POINT('',(28.61,-7.8,-52.11));
#21714=CARTESIAN_POINT('',(28.61,-7.41,-52.5));
#21715=CARTESIAN_POINT('Origin',(19.,1.61,-52.11));
#21716=CARTESIAN_POINT('',(19.39,1.61,-52.5));
#21717=CARTESIAN_POINT('',(19.39,2.,-52.11));
#21718=CARTESIAN_POINT('',(19.39,1.61,-52.5));
#21719=CARTESIAN_POINT('',(19.,1.61,-52.11));
#21720=CARTESIAN_POINT('',(19.,1.61,-52.11));
#21721=CARTESIAN_POINT('',(19.39,2.,-52.11));
#21722=CARTESIAN_POINT('Origin',(28.61,-7.8,-42.89));
#21723=CARTESIAN_POINT('',(28.61,-7.41,-42.5));
#21724=CARTESIAN_POINT('',(29.,-7.41,-42.89));
#21725=CARTESIAN_POINT('',(28.61,-7.41,-42.5));
#21726=CARTESIAN_POINT('',(28.61,-7.8,-42.89));
#21727=CARTESIAN_POINT('',(28.61,-7.8,-42.89));
#21728=CARTESIAN_POINT('',(29.,-7.41,-42.89));
#21729=CARTESIAN_POINT('Origin',(19.39,1.61,-42.5));
#21730=CARTESIAN_POINT('',(19.,1.61,-42.89));
#21731=CARTESIAN_POINT('',(19.39,2.,-42.89));
#21732=CARTESIAN_POINT('',(19.,1.61,-42.89));
#21733=CARTESIAN_POINT('',(19.39,1.61,-42.5));
#21734=CARTESIAN_POINT('',(19.39,1.61,-42.5));
#21735=CARTESIAN_POINT('',(19.39,2.,-42.89));
#21736=CARTESIAN_POINT('Origin',(19.39,-7.8,-52.11));
#21737=CARTESIAN_POINT('',(19.39,-7.41,-52.5));
#21738=CARTESIAN_POINT('',(19.,-7.41,-52.11));
#21739=CARTESIAN_POINT('',(19.39,-7.41,-52.5));
#21740=CARTESIAN_POINT('',(19.39,-7.8,-52.11));
#21741=CARTESIAN_POINT('',(19.39,-7.8,-52.11));
#21742=CARTESIAN_POINT('',(19.,-7.41,-52.11));
#21743=CARTESIAN_POINT('Origin',(26.5,-7.605,-52.305));
#21744=CARTESIAN_POINT('',(26.5,-7.8,-52.11));
#21745=CARTESIAN_POINT('',(26.5,-7.41,-52.5));
#21746=CARTESIAN_POINT('Origin',(19.39,-7.41,-42.5));
#21747=CARTESIAN_POINT('',(19.39,-7.8,-42.89));
#21748=CARTESIAN_POINT('',(19.,-7.41,-42.89));
#21749=CARTESIAN_POINT('',(19.39,-7.8,-42.89));
#21750=CARTESIAN_POINT('',(19.39,-7.41,-42.5));
#21751=CARTESIAN_POINT('',(19.39,-7.41,-42.5));
#21752=CARTESIAN_POINT('',(19.,-7.41,-42.89));
#21753=CARTESIAN_POINT('Origin',(21.5,-7.605,-42.695));
#21754=CARTESIAN_POINT('',(21.5,-7.8,-42.89));
#21755=CARTESIAN_POINT('',(21.5,-7.41,-42.5));
#21756=CARTESIAN_POINT('Origin',(19.195,-7.8,-42.695));
#21757=CARTESIAN_POINT('',(19.,-7.8,-42.89));
#21758=CARTESIAN_POINT('',(19.39,-7.8,-42.5));
#21759=CARTESIAN_POINT('Origin',(19.195,-7.605,-50.));
#21760=CARTESIAN_POINT('',(19.39,-7.8,-50.));
#21761=CARTESIAN_POINT('',(19.,-7.41,-50.));
#21762=CARTESIAN_POINT('Origin',(19.195,-7.8,-52.305));
#21763=CARTESIAN_POINT('',(19.39,-7.8,-52.5));
#21764=CARTESIAN_POINT('',(19.,-7.8,-52.11));
#21765=CARTESIAN_POINT('Origin',(21.5,1.805,-42.695));
#21766=CARTESIAN_POINT('',(21.5,2.,-42.89));
#21767=CARTESIAN_POINT('',(21.5,1.61,-42.5));
#21768=CARTESIAN_POINT('Origin',(19.195,1.805,-50.));
#21769=CARTESIAN_POINT('',(19.39,2.,-50.));
#21770=CARTESIAN_POINT('',(19.,1.61,-50.));
#21771=CARTESIAN_POINT('Origin',(28.805,-7.605,-45.));
#21772=CARTESIAN_POINT('',(28.61,-7.8,-45.));
#21773=CARTESIAN_POINT('',(29.,-7.41,-45.));
#21774=CARTESIAN_POINT('Origin',(28.805,-7.8,-42.695));
#21775=CARTESIAN_POINT('',(28.61,-7.8,-42.5));
#21776=CARTESIAN_POINT('',(29.,-7.8,-42.89));
#21777=CARTESIAN_POINT('Origin',(26.5,1.805,-52.305));
#21778=CARTESIAN_POINT('',(26.5,2.,-52.11));
#21779=CARTESIAN_POINT('',(26.5,1.61,-52.5));
#21780=CARTESIAN_POINT('Origin',(28.805,-7.8,-52.305));
#21781=CARTESIAN_POINT('',(29.,-7.8,-52.11));
#21782=CARTESIAN_POINT('',(28.61,-7.8,-52.5));
#21783=CARTESIAN_POINT('Origin',(28.805,1.805,-45.));
#21784=CARTESIAN_POINT('',(28.61,2.,-45.));
#21785=CARTESIAN_POINT('',(29.,1.61,-45.));
#21786=CARTESIAN_POINT('Origin',(29.,-7.8,-52.5));
#21787=CARTESIAN_POINT('Origin',(19.,-7.8,-42.5));
#21788=CARTESIAN_POINT('Origin',(24.,-7.8,-47.5));
#21789=CARTESIAN_POINT('',(19.95,-7.8,-47.5));
#21790=CARTESIAN_POINT('Origin',(24.,-7.8,-47.5));
#21791=CARTESIAN_POINT('Origin',(19.,-7.8,-52.5));
#21792=CARTESIAN_POINT('Origin',(24.,2.,-47.5));
#21793=CARTESIAN_POINT('',(19.95,2.,-47.5));
#21794=CARTESIAN_POINT('Origin',(24.,2.,-47.5));
#21795=CARTESIAN_POINT('Origin',(29.,-7.8,-42.5));
#21796=CARTESIAN_POINT('Origin',(24.,2.,-47.5));
#21797=CARTESIAN_POINT('',(19.95,2.,-47.5));
#21798=CARTESIAN_POINT('',(0.,0.,0.));
#21799=CARTESIAN_POINT('Origin',(4.7,0.,0.));
#21800=CARTESIAN_POINT('',(-5.40584015536924,-3.95830846622076,0.00274910382348996));
#21801=CARTESIAN_POINT('',(-5.51115984463076,-3.9570708572248,0.00447188352567895));
#21802=CARTESIAN_POINT('',(4.7,-3.954,-4.84225344382863E-16));
#21803=CARTESIAN_POINT('',(-5.646,1.69040986975532,3.57773147777698));
#21804=CARTESIAN_POINT('Ctrl Pts',(-5.40584015536924,-3.95830846622076,
0.00274910382348996));
#21805=CARTESIAN_POINT('Ctrl Pts',(-5.41040414140305,-3.9594161894576,0.153448192401004));
#21806=CARTESIAN_POINT('Ctrl Pts',(-5.41496812743687,-3.9515526888245,0.304023613068971));
#21807=CARTESIAN_POINT('Ctrl Pts',(-5.41953211347068,-3.93433121121586,
0.45351211176479));
#21808=CARTESIAN_POINT('Ctrl Pts',(-5.4591048501247,-3.78500976431612,1.74967492818534));
#21809=CARTESIAN_POINT('Ctrl Pts',(-5.49867758677871,-2.93215360777617,
2.96412271836921));
#21810=CARTESIAN_POINT('Ctrl Pts',(-5.53825032343272,-1.76367516250592,
3.54561744325898));
#21811=CARTESIAN_POINT('Ctrl Pts',(-5.57416688228848,-0.703153995669211,
4.07338709673073));
#21812=CARTESIAN_POINT('Ctrl Pts',(-5.61008344114424,0.617362135119781,
4.07975944947112));
#21813=CARTESIAN_POINT('Ctrl Pts',(-5.646,1.69249901178079,3.58003443294051));
#21814=CARTESIAN_POINT('',(-5.646,-1.6883207277298,3.57542852261347));
#21815=CARTESIAN_POINT('Origin',(-5.646,0.,0.));
#21816=CARTESIAN_POINT('Ctrl Pts',(-5.646,-1.68832072772979,3.57542852261347));
#21817=CARTESIAN_POINT('Ctrl Pts',(-5.60642726334599,-2.87366031862924,
3.01571004745528));
#21818=CARTESIAN_POINT('Ctrl Pts',(-5.56685452669198,-3.74882603463833,
1.82534319022921));
#21819=CARTESIAN_POINT('Ctrl Pts',(-5.52728179003796,-3.92388973907126,
0.534376331785177));
#21820=CARTESIAN_POINT('Ctrl Pts',(-5.52190780823556,-3.94766340855763,
0.359062896542186));
#21821=CARTESIAN_POINT('Ctrl Pts',(-5.51653382643316,-3.95852602877135,
0.18189422941716));
#21822=CARTESIAN_POINT('Ctrl Pts',(-5.51115984463076,-3.9570708572248,0.00447188352567895));
#21823=CARTESIAN_POINT('Origin',(4.7,0.,0.));
#21824=CARTESIAN_POINT('',(-4.65584015536924,-3.94807202781677,0.00139985687555771));
#21825=CARTESIAN_POINT('',(-4.76115984463076,-3.94781927952859,0.001010842389746));
#21826=CARTESIAN_POINT('',(4.7,-3.954,-4.84225344382863E-16));
#21827=CARTESIAN_POINT('Ctrl Pts',(-4.65584015536924,-3.94807202781677,
0.00139985687555771));
#21828=CARTESIAN_POINT('Ctrl Pts',(-4.67296772147897,-3.94988746363517,
0.570738284822051));
#21829=CARTESIAN_POINT('Ctrl Pts',(-4.69009528758871,-3.83478261226913,
1.1393760863107));
#21830=CARTESIAN_POINT('Ctrl Pts',(-4.70722285369845,-3.599099248183,1.65264375078517));
#21831=CARTESIAN_POINT('Ctrl Pts',(-4.74679559035246,-3.05455978233268,
2.83853356076355));
#21832=CARTESIAN_POINT('Ctrl Pts',(-4.78636832700647,-1.86633917166041,
3.72884240545855));
#21833=CARTESIAN_POINT('Ctrl Pts',(-4.82594106366049,-0.575235943424667,
3.91838868771338));
#21834=CARTESIAN_POINT('Ctrl Pts',(-4.8655138003145,0.715867284811076,4.10793496996821));
#21835=CARTESIAN_POINT('Ctrl Pts',(-4.90508653696851,2.10985313061029,3.59671868978285));
#21836=CARTESIAN_POINT('Ctrl Pts',(-4.94465927362253,2.97225595093563,2.61735378803508));
#21837=CARTESIAN_POINT('Ctrl Pts',(-4.98423201027654,3.83465877126098,1.6379888862873));
#21838=CARTESIAN_POINT('Ctrl Pts',(-5.02380474693055,4.16547856611245,0.190475362977117));
#21839=CARTESIAN_POINT('Ctrl Pts',(-5.06337748358456,3.81416626107115,-1.06625514220163));
#21840=CARTESIAN_POINT('Ctrl Pts',(-5.10295022023858,3.46285395602986,-2.32298564738038));
#21841=CARTESIAN_POINT('Ctrl Pts',(-5.14252295689259,2.42940955109579,-3.38893313442769));
#21842=CARTESIAN_POINT('Ctrl Pts',(-5.1820956935466,1.18415546882936,-3.77916117270054));
#21843=CARTESIAN_POINT('Ctrl Pts',(-5.22166843020061,-0.0610986134370675,
-4.16938921097339));
#21844=CARTESIAN_POINT('Ctrl Pts',(-5.26124116685463,-1.51816237303585,
-3.88389780047179));
#21845=CARTESIAN_POINT('Ctrl Pts',(-5.30081390350864,-2.52380088420549,
-3.05221317389238));
#21846=CARTESIAN_POINT('Ctrl Pts',(-5.33582265412884,-3.41345752229485,
-2.31644804495686));
#21847=CARTESIAN_POINT('Ctrl Pts',(-5.37083140474904,-3.94981150626788,
-1.15321122813476));
#21848=CARTESIAN_POINT('Ctrl Pts',(-5.40584015536924,-3.95830846622076,
0.00274910382348996));
#21849=CARTESIAN_POINT('Ctrl Pts',(-5.51115984463076,-3.9570708572248,0.00447188352567895));
#21850=CARTESIAN_POINT('Ctrl Pts',(-5.47696108977915,-3.94781048813209,
-1.12460215048567));
#21851=CARTESIAN_POINT('Ctrl Pts',(-5.44276233492753,-3.43971035750927,
-2.26394954012984));
#21852=CARTESIAN_POINT('Ctrl Pts',(-5.40856358007592,-2.58566274428266,
-3.00082354295664));
#21853=CARTESIAN_POINT('Ctrl Pts',(-5.36899084342191,-1.59741035220436,
-3.85348969959244));
#21854=CARTESIAN_POINT('Ctrl Pts',(-5.3294181067679,-0.145943875190994,
-4.16725515320204));
#21855=CARTESIAN_POINT('Ctrl Pts',(-5.28984537011389,1.10711897366749,-3.80213656168223));
#21856=CARTESIAN_POINT('Ctrl Pts',(-5.25027263345987,2.36018182252598,-3.43701797016241));
#21857=CARTESIAN_POINT('Ctrl Pts',(-5.21069989680586,3.41484104322959,-2.39301533351318));
#21858=CARTESIAN_POINT('Ctrl Pts',(-5.17112716015184,3.79159857088148,-1.14386006663144));
#21859=CARTESIAN_POINT('Ctrl Pts',(-5.13155442349783,4.16835609853338,0.105295200250295));
#21860=CARTESIAN_POINT('Ctrl Pts',(-5.09198168684382,3.86721193313355,1.55960309736453));
#21861=CARTESIAN_POINT('Ctrl Pts',(-5.0524089501898,3.02495731201586,2.55640561878531));
#21862=CARTESIAN_POINT('Ctrl Pts',(-5.01283621353579,2.18270269089815,3.5532081402061));
#21863=CARTESIAN_POINT('Ctrl Pts',(-4.97326347688178,0.799337614062568,
4.09250528593342));
#21864=CARTESIAN_POINT('Ctrl Pts',(-4.93369074022777,-0.495374153645519,
3.92923511481126));
#21865=CARTESIAN_POINT('Ctrl Pts',(-4.89411800357376,-1.7900859213536,3.76596494368911));
#21866=CARTESIAN_POINT('Ctrl Pts',(-4.85454526691974,-2.99614437993419,
2.9001274557175));
#21867=CARTESIAN_POINT('Ctrl Pts',(-4.81497253026573,-3.5647017355765,1.72559158222104));
#21868=CARTESIAN_POINT('Ctrl Pts',(-4.7970349683874,-3.82241787073735,1.19319701741357));
#21869=CARTESIAN_POINT('Ctrl Pts',(-4.77909740650908,-3.94915080627378,
0.597376205861484));
#21870=CARTESIAN_POINT('Ctrl Pts',(-4.76115984463076,-3.94781927952859,
0.001010842389746));
#21871=CARTESIAN_POINT('Origin',(4.7,0.,0.));
#21872=CARTESIAN_POINT('',(-3.90584015536924,-3.95333922947531,-0.00355421683578439));
#21873=CARTESIAN_POINT('',(-4.01115984463076,-3.95413953703022,-0.00354925354858068));
#21874=CARTESIAN_POINT('',(4.7,-3.954,-4.84225344382863E-16));
#21875=CARTESIAN_POINT('Ctrl Pts',(-3.90584015536924,-3.95333922947531,
-0.00355421683578439));
#21876=CARTESIAN_POINT('Ctrl Pts',(-3.9355313015549,-3.94453230977388,0.980091333856488));
#21877=CARTESIAN_POINT('Ctrl Pts',(-3.96522244774056,-3.57263269613905,
1.96968142938521));
#21878=CARTESIAN_POINT('Ctrl Pts',(-3.99491359392622,-2.90796156736813,
2.68858637312984));
#21879=CARTESIAN_POINT('Ctrl Pts',(-4.03448633058023,-2.02207944695739,
3.64675201079778));
#21880=CARTESIAN_POINT('Ctrl Pts',(-4.07405906723424,-0.616121026144095,
4.12407533616519));
#21881=CARTESIAN_POINT('Ctrl Pts',(-4.11363180388825,0.670009230171976,
3.90330920884321));
#21882=CARTESIAN_POINT('Ctrl Pts',(-4.15320454054227,1.95613948648805,3.68254308152123));
#21883=CARTESIAN_POINT('Ctrl Pts',(-4.19277727719628,3.12244157830689,2.76368750150988));
#21884=CARTESIAN_POINT('Ctrl Pts',(-4.23235001385029,3.63808732338842,1.56494695195733));
#21885=CARTESIAN_POINT('Ctrl Pts',(-4.27192275050431,4.15373306846994,0.366206402404782));
#21886=CARTESIAN_POINT('Ctrl Pts',(-4.31149548715832,4.01872246681414,-1.11241911668896));
#21887=CARTESIAN_POINT('Ctrl Pts',(-4.35106822381233,3.29450433464159,-2.19794909096417));
#21888=CARTESIAN_POINT('Ctrl Pts',(-4.39064096046634,2.57028620246903,-3.28347906523937));
#21889=CARTESIAN_POINT('Ctrl Pts',(-4.43021369712036,1.25686053977973,-3.97591349469604));
#21890=CARTESIAN_POINT('Ctrl Pts',(-4.46978643377437,-0.0479839970950056,
-3.96010399035171));
#21891=CARTESIAN_POINT('Ctrl Pts',(-4.50935917042838,-1.35282853396974,
-3.94429448600738));
#21892=CARTESIAN_POINT('Ctrl Pts',(-4.5489319070824,-2.64909194502991,-3.22024104786205));
#21893=CARTESIAN_POINT('Ctrl Pts',(-4.58850464373641,-3.3467944900458,-2.1174789411585));
#21894=CARTESIAN_POINT('Ctrl Pts',(-4.61094981428069,-3.74252281050475,
-1.49200580870543));
#21895=CARTESIAN_POINT('Ctrl Pts',(-4.63339498482496,-3.94569295268753,
-0.744701371448065));
#21896=CARTESIAN_POINT('Ctrl Pts',(-4.65584015536924,-3.94807202781677,
0.00139985687555771));
#21897=CARTESIAN_POINT('Ctrl Pts',(-4.76115984463076,-3.94781927952859,
0.001010842389746));
#21898=CARTESIAN_POINT('Ctrl Pts',(-4.73952466985507,-3.94621327454049,
-0.718288076627242));
#21899=CARTESIAN_POINT('Ctrl Pts',(-4.71788949507938,-3.75830307984049,
-1.43837919281071));
#21900=CARTESIAN_POINT('Ctrl Pts',(-4.69625432030369,-3.3892100636415,-2.04892701679288));
#21901=CARTESIAN_POINT('Ctrl Pts',(-4.65668158364968,-2.71410478336013,
-3.16567548328903));
#21902=CARTESIAN_POINT('Ctrl Pts',(-4.61710884699566,-1.43283797009337,
-3.91593815726002));
#21903=CARTESIAN_POINT('Ctrl Pts',(-4.57753611034165,-0.128583036525032,
-3.95829929255482));
#21904=CARTESIAN_POINT('Ctrl Pts',(-4.53796337368764,1.1756718970433,-4.00066042784961));
#21905=CARTESIAN_POINT('Ctrl Pts',(-4.49839063703363,2.50291495091321,-3.33512002446819));
#21906=CARTESIAN_POINT('Ctrl Pts',(-4.45881790037961,3.24907874340357,-2.26456057724478));
#21907=CARTESIAN_POINT('Ctrl Pts',(-4.4192451637256,3.99524253589392,-1.19400113002136));
#21908=CARTESIAN_POINT('Ctrl Pts',(-4.37967242707158,4.16032706700472,0.281577361044059));
#21909=CARTESIAN_POINT('Ctrl Pts',(-4.34009969041757,3.66919043867727,1.49056783765062));
#21910=CARTESIAN_POINT('Ctrl Pts',(-4.30052695376356,3.17805381034982,2.69955831425719));
#21911=CARTESIAN_POINT('Ctrl Pts',(-4.26095421710955,2.03069602258413,3.6419607764049));
#21912=CARTESIAN_POINT('Ctrl Pts',(-4.22138148045554,0.749325781401231,
3.88886069412444));
#21913=CARTESIAN_POINT('Ctrl Pts',(-4.18180874380152,-0.532044459781662,
4.13576061184399));
#21914=CARTESIAN_POINT('Ctrl Pts',(-4.14223600714751,-1.94742715438175,
3.68715798513539));
#21915=CARTESIAN_POINT('Ctrl Pts',(-4.1026632704935,-2.85262996255091,2.74722438990827));
#21916=CARTESIAN_POINT('Ctrl Pts',(-4.07216212853925,-3.550325438877,2.02275975997274));
#21917=CARTESIAN_POINT('Ctrl Pts',(-4.04166098658501,-3.94493666981705,
1.00640852339343));
#21918=CARTESIAN_POINT('Ctrl Pts',(-4.01115984463076,-3.95413953703022,
-0.00354925354858068));
#21919=CARTESIAN_POINT('Origin',(4.7,0.,0.));
#21920=CARTESIAN_POINT('',(-3.15584015536924,-3.95962261149855,0.00156596972554903));
#21921=CARTESIAN_POINT('',(-3.26115984463076,-3.9591353959144,0.00198372275667011));
#21922=CARTESIAN_POINT('',(4.7,-3.954,-4.84225344382863E-16));
#21923=CARTESIAN_POINT('Ctrl Pts',(-3.15584015536924,-3.95962261149855,
0.00156596972554903));
#21924=CARTESIAN_POINT('Ctrl Pts',(-3.15852214497681,-3.96007009395101,
0.0900527454151371));
#21925=CARTESIAN_POINT('Ctrl Pts',(-3.16120413458437,-3.95735922725396,
0.178511619278897));
#21926=CARTESIAN_POINT('Ctrl Pts',(-3.16388612419194,-3.951402336726,0.26675136050462));
#21927=CARTESIAN_POINT('Ctrl Pts',(-3.20345886084596,-3.86350846141984,
1.56872808408672));
#21928=CARTESIAN_POINT('Ctrl Pts',(-3.24303159749997,-3.06892337125733,
2.82299748379964));
#21929=CARTESIAN_POINT('Ctrl Pts',(-3.28260433415398,-1.92929263952253,
3.4586943546257));
#21930=CARTESIAN_POINT('Ctrl Pts',(-3.32217707080799,-0.789661907787753,
4.09439122545175));
#21931=CARTESIAN_POINT('Ctrl Pts',(-3.36174980746201,0.695014465519304,
4.11151556739096));
#21932=CARTESIAN_POINT('Ctrl Pts',(-3.40132254411602,1.84900440207876,3.50227346215549));
#21933=CARTESIAN_POINT('Ctrl Pts',(-3.44089528077003,3.00299433863823,2.89303135692001));
#21934=CARTESIAN_POINT('Ctrl Pts',(-3.48046801742405,3.82629783845009,1.65742280450983));
#21935=CARTESIAN_POINT('Ctrl Pts',(-3.52004075407806,3.94419849611561,0.357819722064362));
#21936=CARTESIAN_POINT('Ctrl Pts',(-3.55961349073207,4.06209915378113,-0.941783360381109));
#21937=CARTESIAN_POINT('Ctrl Pts',(-3.59918622738609,3.47459696930029,-2.30538097286188));
#21938=CARTESIAN_POINT('Ctrl Pts',(-3.6387589640401,2.4490863012015,-3.11234848363658));
#21939=CARTESIAN_POINT('Ctrl Pts',(-3.67833170069411,1.4235756331027,-3.91931599441128));
#21940=CARTESIAN_POINT('Ctrl Pts',(-3.71790443734813,-0.0399435186140502,
-4.16965340347993));
#21941=CARTESIAN_POINT('Ctrl Pts',(-3.75747717400214,-1.27536853738317,
-3.74942283333533));
#21942=CARTESIAN_POINT('Ctrl Pts',(-3.79704991065615,-2.51079355615229,
-3.32919226319073));
#21943=CARTESIAN_POINT('Ctrl Pts',(-3.83662264731016,-3.51812444197377,
-2.23839371383289));
#21944=CARTESIAN_POINT('Ctrl Pts',(-3.87619538396417,-3.83888697488042,
-0.973490464169738));
#21945=CARTESIAN_POINT('Ctrl Pts',(-3.88607697443253,-3.91898363373643,
-0.657635232712209));
#21946=CARTESIAN_POINT('Ctrl Pts',(-3.89595856490088,-3.95627028418209,
-0.330923946423857));
#21947=CARTESIAN_POINT('Ctrl Pts',(-3.90584015536924,-3.95333922947531,
-0.00355421683578439));
#21948=CARTESIAN_POINT('Ctrl Pts',(-4.01115984463076,-3.95413953703022,
-0.00354925354858068));
#21949=CARTESIAN_POINT('Ctrl Pts',(-4.00208824993099,-3.95687663722007,
-0.303929076377534));
#21950=CARTESIAN_POINT('Ctrl Pts',(-3.99301665523123,-3.92552144433661,
-0.603743349207523));
#21951=CARTESIAN_POINT('Ctrl Pts',(-3.98394506053146,-3.85790810174668,
-0.895144652921099));
#21952=CARTESIAN_POINT('Ctrl Pts',(-3.94437232387744,-3.56296051103506,
-2.16631553677773));
#21953=CARTESIAN_POINT('Ctrl Pts',(-3.90479958722343,-2.57804240787361,
-3.27739274074537));
#21954=CARTESIAN_POINT('Ctrl Pts',(-3.86522685056942,-1.35142751700913,
-3.72268442840996));
#21955=CARTESIAN_POINT('Ctrl Pts',(-3.82565411391541,-0.12481262614466,
-4.16797611607455));
#21956=CARTESIAN_POINT('Ctrl Pts',(-3.78608137726139,1.34349905242283,-3.94748228743609));
#21957=CARTESIAN_POINT('Ctrl Pts',(-3.74650864060738,2.3852238560361,-3.16155734667935));
#21958=CARTESIAN_POINT('Ctrl Pts',(-3.70693590395337,3.42694865964938,-2.37563240592262));
#21959=CARTESIAN_POINT('Ctrl Pts',(-3.66736316729935,4.04208658830845,-1.02427635304761));
#21960=CARTESIAN_POINT('Ctrl Pts',(-3.62779043064534,3.95066510436862,0.27745749225628));
#21961=CARTESIAN_POINT('Ctrl Pts',(-3.58821769399133,3.85924362042878,1.57919133756016));
#21962=CARTESIAN_POINT('Ctrl Pts',(-3.54864495733732,3.06126272389006,2.83130297529291));
#21963=CARTESIAN_POINT('Ctrl Pts',(-3.5090722206833,1.91991360954393,3.4639094616809));
#21964=CARTESIAN_POINT('Ctrl Pts',(-3.46949948402929,0.7785644951978,4.09651594806888));
#21965=CARTESIAN_POINT('Ctrl Pts',(-3.42992674737528,-0.706152836955741,
4.10961728311208));
#21966=CARTESIAN_POINT('Ctrl Pts',(-3.39035401072126,-1.85848769767767,
3.49725046416115));
#21967=CARTESIAN_POINT('Ctrl Pts',(-3.35078127406725,-3.01082255839962,
2.88488364521021));
#21968=CARTESIAN_POINT('Ctrl Pts',(-3.31120853741323,-3.83077494768995,
1.64704867226511));
#21969=CARTESIAN_POINT('Ctrl Pts',(-3.27163580075922,-3.94515366365166,
0.347130865392129));
#21970=CARTESIAN_POINT('Ctrl Pts',(-3.26814381538307,-3.95524669327894,
0.232423257184699));
#21971=CARTESIAN_POINT('Ctrl Pts',(-3.26465183000691,-3.95984564225403,
0.117232229442771));
#21972=CARTESIAN_POINT('Ctrl Pts',(-3.26115984463076,-3.9591353959144,0.00198372275667011));
#21973=CARTESIAN_POINT('Origin',(4.7,0.,0.));
#21974=CARTESIAN_POINT('',(-2.40584015536924,-3.94895503742539,0.00226341524845186));
#21975=CARTESIAN_POINT('',(-2.51115984463076,-3.94852321086993,0.00190807621368246));
#21976=CARTESIAN_POINT('',(4.7,-3.954,-4.84225344382863E-16));
#21977=CARTESIAN_POINT('Ctrl Pts',(-2.40584015536924,-3.94895503742539,
0.00226341524845186));
#21978=CARTESIAN_POINT('Ctrl Pts',(-2.42108572505273,-3.95161164091452,
0.508757332831716));
#21979=CARTESIAN_POINT('Ctrl Pts',(-2.43633129473622,-3.86116503322235,
1.0143385318084));
#21980=CARTESIAN_POINT('Ctrl Pts',(-2.45157686441971,-3.67321498688243,
1.48061756513418));
#21981=CARTESIAN_POINT('Ctrl Pts',(-2.49114960107372,-3.18535537636404,
2.69093228450277));
#21982=CARTESIAN_POINT('Ctrl Pts',(-2.53072233772774,-2.04055715558632,
3.63644495749262));
#21983=CARTESIAN_POINT('Ctrl Pts',(-2.57029507438175,-0.759861069646289,
3.88681719010075));
#21984=CARTESIAN_POINT('Ctrl Pts',(-2.60986781103576,0.520835016293738,
4.13718942270888));
#21985=CARTESIAN_POINT('Ctrl Pts',(-2.64944054768977,1.93742896739607,3.69242121493529));
#21986=CARTESIAN_POINT('Ctrl Pts',(-2.68901328434379,2.84517557503799,2.75494331352305));
#21987=CARTESIAN_POINT('Ctrl Pts',(-2.7285860209978,3.7529221826799,1.81746541211081));
#21988=CARTESIAN_POINT('Ctrl Pts',(-2.76815875765182,4.15182144686141,0.387277817059935));
#21989=CARTESIAN_POINT('Ctrl Pts',(-2.80773149430583,3.86031930315829,-0.884687284678487));
#21990=CARTESIAN_POINT('Ctrl Pts',(-2.84730423095984,3.56881715945518,-2.15665238641692));
#21991=CARTESIAN_POINT('Ctrl Pts',(-2.88687696761385,2.58691360786742,-3.27039499484289));
#21992=CARTESIAN_POINT('Ctrl Pts',(-2.92644970426786,1.3615099005383,-3.71900894150773));
#21993=CARTESIAN_POINT('Ctrl Pts',(-2.96602244092188,0.136106193209184,
-4.16762288817257));
#21994=CARTESIAN_POINT('Ctrl Pts',(-3.00559517757589,-1.3327976698613,-3.95110817307629));
#21995=CARTESIAN_POINT('Ctrl Pts',(-3.0451679142299,-2.37664827117163,-3.16800879180251));
#21996=CARTESIAN_POINT('Ctrl Pts',(-3.08205866127635,-3.34975328596754,
-2.43798292982139));
#21997=CARTESIAN_POINT('Ctrl Pts',(-3.11894940832279,-3.95346749370281,
-1.21556896983858));
#21998=CARTESIAN_POINT('Ctrl Pts',(-3.15584015536924,-3.95962261149855,
0.00156596972554903));
#21999=CARTESIAN_POINT('Ctrl Pts',(-3.26115984463076,-3.9591353959144,0.00198372275667011));
#22000=CARTESIAN_POINT('Ctrl Pts',(-3.2250790933529,-3.9517968137711,-1.18881528037774));
#22001=CARTESIAN_POINT('Ctrl Pts',(-3.18899834207504,-3.37765148143732,
-2.38575070374499));
#22002=CARTESIAN_POINT('Ctrl Pts',(-3.15291759079718,-2.44064387050199,
-3.11897334347904));
#22003=CARTESIAN_POINT('Ctrl Pts',(-3.11334485414317,-1.41295031875755,
-3.92315910467638));
#22004=CARTESIAN_POINT('Ctrl Pts',(-3.07377211748916,0.051241827364419,
-4.16952998627021));
#22005=CARTESIAN_POINT('Ctrl Pts',(-3.03419938083514,1.28552363453667,-3.74595331657321));
#22006=CARTESIAN_POINT('Ctrl Pts',(-2.99462664418113,2.51980544170892,-3.32237664687621));
#22007=CARTESIAN_POINT('Ctrl Pts',(-2.95505390752712,3.52417690993145,-2.22885242588837));
#22008=CARTESIAN_POINT('Ctrl Pts',(-2.91548117087311,3.84151079044162,-0.963084679153289));
#22009=CARTESIAN_POINT('Ctrl Pts',(-2.87590843421909,4.15884467095179,0.302683067581793));
#22010=CARTESIAN_POINT('Ctrl Pts',(-2.83633569756508,3.78914096374961,1.74069434006411));
#22011=CARTESIAN_POINT('Ctrl Pts',(-2.79676296091107,2.90066573799585,2.69645610450251));
#22012=CARTESIAN_POINT('Ctrl Pts',(-2.75719022425705,2.01219051224209,3.6522178689409));
#22013=CARTESIAN_POINT('Ctrl Pts',(-2.71761748760304,0.604943767936768,
4.12573012533537));
#22014=CARTESIAN_POINT('Ctrl Pts',(-2.67804475094903,-0.680583552468711,
3.90147962722707));
#22015=CARTESIAN_POINT('Ctrl Pts',(-2.63847201429502,-1.96611087287421,
3.67722912911877));
#22016=CARTESIAN_POINT('Ctrl Pts',(-2.598899277641,-3.12991876937986,2.75521587650767));
#22017=CARTESIAN_POINT('Ctrl Pts',(-2.55932654098699,-3.64231447785219,
1.55508279384779));
#22018=CARTESIAN_POINT('Ctrl Pts',(-2.54327097553491,-3.85020515032875,
1.06816131989674));
#22019=CARTESIAN_POINT('Ctrl Pts',(-2.52721541008284,-3.95086616481225,
0.535458242830061));
#22020=CARTESIAN_POINT('Ctrl Pts',(-2.51115984463076,-3.94852321086993,
0.00190807621368246));
#22021=CARTESIAN_POINT('Origin',(4.7,0.,0.));
#22022=CARTESIAN_POINT('',(-1.65584015536924,-3.95156722446408,-0.00334773101343278));
#22023=CARTESIAN_POINT('',(-1.76115984463076,-3.95230955109532,-0.00347299664959956));
#22024=CARTESIAN_POINT('',(4.7,-3.954,-4.84225344382863E-16));
#22025=CARTESIAN_POINT('Ctrl Pts',(-1.65584015536924,-3.95156722446408,
-0.00334773101343277));
#22026=CARTESIAN_POINT('Ctrl Pts',(-1.68364930512865,-3.94407310588175,
0.918999373347058));
#22027=CARTESIAN_POINT('Ctrl Pts',(-1.71145845488806,-3.62183865226459,
1.84606618164852));
#22028=CARTESIAN_POINT('Ctrl Pts',(-1.73926760464748,-3.03183124106019,
2.54808477877248));
#22029=CARTESIAN_POINT('Ctrl Pts',(-1.77884034130149,-2.19224397897198,
3.54706523342667));
#22030=CARTESIAN_POINT('Ctrl Pts',(-1.8184130779555,-0.810426814979439,
4.09033174829379));
#22031=CARTESIAN_POINT('Ctrl Pts',(-1.85798581460952,0.484703266587122,
3.93062329121606));
#22032=CARTESIAN_POINT('Ctrl Pts',(-1.89755855126353,1.77983334815371,3.77091483413833));
#22033=CARTESIAN_POINT('Ctrl Pts',(-1.93713128791754,2.98827634729431,2.90823140511572));
#22034=CARTESIAN_POINT('Ctrl Pts',(-1.97670402457155,3.56002438557403,1.73521269249398));
#22035=CARTESIAN_POINT('Ctrl Pts',(-2.01627676122557,4.13177242385376,0.562193979872254));
#22036=CARTESIAN_POINT('Ctrl Pts',(-2.05584949787958,4.06682550127261,-0.921160016348606));
#22037=CARTESIAN_POINT('Ctrl Pts',(-2.09542223453359,3.39474340602312,-2.03971907902412));
#22038=CARTESIAN_POINT('Ctrl Pts',(-2.13499497118761,2.72266131077363,-3.15827814169962));
#22039=CARTESIAN_POINT('Ctrl Pts',(-2.17456770784162,1.4434440428558,-3.91204227082979));
#22040=CARTESIAN_POINT('Ctrl Pts',(-2.21414044449563,0.139311513420746,
-3.95794504968973));
#22041=CARTESIAN_POINT('Ctrl Pts',(-2.25371318114964,-1.16482101601431,
-4.00384782854967));
#22042=CARTESIAN_POINT('Ctrl Pts',(-2.29328591780366,-2.49386880696661,
-3.34188925713937));
#22043=CARTESIAN_POINT('Ctrl Pts',(-2.33285865445767,-3.24293220231323,
-2.27335158856057));
#22044=CARTESIAN_POINT('Ctrl Pts',(-2.35718582142819,-3.70341565205352,
-1.61647272508745));
#22045=CARTESIAN_POINT('Ctrl Pts',(-2.38151298839871,-3.94471592809748,
-0.805942664183553));
#22046=CARTESIAN_POINT('Ctrl Pts',(-2.40584015536924,-3.94895503742539,
0.00226341524845186));
#22047=CARTESIAN_POINT('Ctrl Pts',(-2.51115984463076,-3.94852321086993,
0.00190807621368246));
#22048=CARTESIAN_POINT('Ctrl Pts',(-2.48764267342882,-3.9450914009381,-0.77960227610563));
#22049=CARTESIAN_POINT('Ctrl Pts',(-2.46412550222689,-3.72066944546383,
-1.56293001901423));
#22050=CARTESIAN_POINT('Ctrl Pts',(-2.44060833102495,-3.28853666992144,
-2.20686742270246));
#22051=CARTESIAN_POINT('Ctrl Pts',(-2.40103559437094,-2.56137963307938,
-3.2904316438842));
#22052=CARTESIAN_POINT('Ctrl Pts',(-2.36146285771693,-1.24608203895624,
-3.979307173539));
#22053=CARTESIAN_POINT('Ctrl Pts',(-2.32189012106291,0.058714687369509,
-3.95996083783634));
#22054=CARTESIAN_POINT('Ctrl Pts',(-2.2823173844089,1.36351141369524,-3.94061450213368));
#22055=CARTESIAN_POINT('Ctrl Pts',(-2.24274464775489,2.6578072722236,-3.21304630107356));
#22056=CARTESIAN_POINT('Ctrl Pts',(-2.20317191110087,3.3525195178114,-2.10839989898019));
#22057=CARTESIAN_POINT('Ctrl Pts',(-2.16359917444686,4.04723176339921,-1.0037534968868));
#22058=CARTESIAN_POINT('Ctrl Pts',(-2.12402643779285,4.14236039604643,0.477971106239855));
#22059=CARTESIAN_POINT('Ctrl Pts',(-2.08445370113883,3.59460879570253,1.6623852914272));
#22060=CARTESIAN_POINT('Ctrl Pts',(-2.04488096448482,3.04685719535864,2.84679947661452));
#22061=CARTESIAN_POINT('Ctrl Pts',(-2.00530822783081,1.85622536202364,3.73390324386254));
#22062=CARTESIAN_POINT('Ctrl Pts',(-1.9657354911768,0.564614642387913,3.91994229001148));
#22063=CARTESIAN_POINT('Ctrl Pts',(-1.92616275452278,-0.72699607724783,
4.10598133616041));
#22064=CARTESIAN_POINT('Ctrl Pts',(-1.88659001786877,-2.1195856831843,3.59095566121024));
#22065=CARTESIAN_POINT('Ctrl Pts',(-1.84701728121476,-2.97933424742549,
2.60927282848582));
#22066=CARTESIAN_POINT('Ctrl Pts',(-1.81839813568676,-3.60110750239726,
1.89931627183638));
#22067=CARTESIAN_POINT('Ctrl Pts',(-1.78977899015876,-3.94419240060798,
0.94528708133517));
#22068=CARTESIAN_POINT('Ctrl Pts',(-1.76115984463076,-3.95230955109532,
-0.00347299664959956));
#22069=CARTESIAN_POINT('Origin',(4.7,0.,0.));
#22070=CARTESIAN_POINT('',(-0.905840155369234,-3.960321004907,0.000484847720224144));
#22071=CARTESIAN_POINT('',(-1.01115984463075,-3.9601030984513,0.000964724550051354));
#22072=CARTESIAN_POINT('',(4.7,-3.954,-4.84225344382863E-16));
#22073=CARTESIAN_POINT('Ctrl Pts',(-0.905840155369234,-3.960321004907,0.000484847720224144));
#22074=CARTESIAN_POINT('Ctrl Pts',(-0.906640148550558,-3.96036688714869,
0.0268665595925369));
#22075=CARTESIAN_POINT('Ctrl Pts',(-0.907440141731881,-3.96012592613957,
0.0532474112658711));
#22076=CARTESIAN_POINT('Ctrl Pts',(-0.908240134913205,-3.95959555770559,
0.0796224433230482));
#22077=CARTESIAN_POINT('Ctrl Pts',(-0.947812871567218,-3.93336017113319,
1.38429881083044));
#22078=CARTESIAN_POINT('Ctrl Pts',(-0.987385608221231,-3.19896824808949,
2.67473504879244));
#22079=CARTESIAN_POINT('Ctrl Pts',(-1.02695834487524,-2.09066918537765,
3.36360507066375));
#22080=CARTESIAN_POINT('Ctrl Pts',(-1.06653108152926,-0.982370122665806,
4.05247509253507));
#22081=CARTESIAN_POINT('Ctrl Pts',(-1.10610381818327,0.499836079714179,
4.13977889831569));
#22082=CARTESIAN_POINT('Ctrl Pts',(-1.14567655483728,1.68134160877037,3.58578124105477));
#22083=CARTESIAN_POINT('Ctrl Pts',(-1.1852492914913,2.86284713782654,3.03178358379385));
#22084=CARTESIAN_POINT('Ctrl Pts',(-1.22482202814531,3.74365199355893,1.83648446349142));
#22085=CARTESIAN_POINT('Ctrl Pts',(-1.26439476479932,3.92286874448592,0.543909484765631));
#22086=CARTESIAN_POINT('Ctrl Pts',(-1.30396750145333,4.1020854954129,-0.748665493960175));
#22087=CARTESIAN_POINT('Ctrl Pts',(-1.34354023810735,3.57971414153446,-2.13851633110934));
#22088=CARTESIAN_POINT('Ctrl Pts',(-1.38311297476136,2.5935055410265,-2.99306961541944));
#22089=CARTESIAN_POINT('Ctrl Pts',(-1.42268571141537,1.60729694051856,-3.84762289972953));
#22090=CARTESIAN_POINT('Ctrl Pts',(-1.46225844806939,0.157251093381126,
-4.16687863120059));
#22091=CARTESIAN_POINT('Ctrl Pts',(-1.5018311847234,-1.09666157514756,-3.80553151395158));
#22092=CARTESIAN_POINT('Ctrl Pts',(-1.54140392137741,-2.35057424367627,
-3.44418439670257));
#22093=CARTESIAN_POINT('Ctrl Pts',(-1.58097665803143,-3.40835373359622,
-2.40223443073346));
#22094=CARTESIAN_POINT('Ctrl Pts',(-1.62054939468544,-3.78856479846426,
-1.15391225052825));
#22095=CARTESIAN_POINT('Ctrl Pts',(-1.63231298158004,-3.90158821503936,
-0.782829841755529));
#22096=CARTESIAN_POINT('Ctrl Pts',(-1.64407656847464,-3.95473732192856,
-0.393511055063059));
#22097=CARTESIAN_POINT('Ctrl Pts',(-1.65584015536924,-3.95156722446408,
-0.00334773101343277));
#22098=CARTESIAN_POINT('Ctrl Pts',(-1.76115984463076,-3.95230955109532,
-0.00347299664959956));
#22099=CARTESIAN_POINT('Ctrl Pts',(-1.75020625350475,-3.95541628073054,
-0.366598092776724));
#22100=CARTESIAN_POINT('Ctrl Pts',(-1.73925266237873,-3.90945451756587,
-0.728951331280733));
#22101=CARTESIAN_POINT('Ctrl Pts',(-1.72829907125272,-3.81126890115824,
-1.07655311732514));
#22102=CARTESIAN_POINT('Ctrl Pts',(-1.68872633459871,-3.45654746810388,
-2.33235623991302));
#22103=CARTESIAN_POINT('Ctrl Pts',(-1.64915359794469,-2.42019707944922,
-3.39562249459013));
#22104=CARTESIAN_POINT('Ctrl Pts',(-1.60958086129068,-1.17389979134669,
-3.78241940181823));
#22105=CARTESIAN_POINT('Ctrl Pts',(-1.57000812463667,0.0723974967558526,
-4.16921630904633));
#22106=CARTESIAN_POINT('Ctrl Pts',(-1.53043538798265,1.52864168430628,-3.87954386882542));
#22107=CARTESIAN_POINT('Ctrl Pts',(-1.49086265132864,2.53204124812124,-3.04524290807442));
#22108=CARTESIAN_POINT('Ctrl Pts',(-1.45128991467463,3.5354408119362,-2.21094194732342));
#22109=CARTESIAN_POINT('Ctrl Pts',(-1.41171717802061,4.08599575201568,-0.832012466042327));
#22110=CARTESIAN_POINT('Ctrl Pts',(-1.3721444413666,3.93312779965345,0.463942844496236));
#22111=CARTESIAN_POINT('Ctrl Pts',(-1.33257170471259,3.78025984729122,1.75989815503479));
#22112=CARTESIAN_POINT('Ctrl Pts',(-1.29299896805858,2.92396900248728,2.97287929483081));
#22113=CARTESIAN_POINT('Ctrl Pts',(-1.25342623140456,1.75398544797205,3.55081290688068));
#22114=CARTESIAN_POINT('Ctrl Pts',(-1.21385349475055,0.584001893456819,
4.12874651893055));
#22115=CARTESIAN_POINT('Ctrl Pts',(-1.17428075809654,-0.899674370769732,
4.07163260323425));
#22116=CARTESIAN_POINT('Ctrl Pts',(-1.13470802144252,-2.02176645125577,
3.40546585182457));
#22117=CARTESIAN_POINT('Ctrl Pts',(-1.09513528478851,-3.14385853174181,
2.73929910041489));
#22118=CARTESIAN_POINT('Ctrl Pts',(-1.0555625481345,-3.90436642848736,1.46407951329185));
#22119=CARTESIAN_POINT('Ctrl Pts',(-1.01598981148048,-3.95715438240394,
0.160207506653819));
#22120=CARTESIAN_POINT('Ctrl Pts',(-1.01437982253057,-3.95930202317079,
0.107160391385077));
#22121=CARTESIAN_POINT('Ctrl Pts',(-1.01276983358066,-3.96027823741067,
0.0540658502883357));
#22122=CARTESIAN_POINT('Ctrl Pts',(-1.01115984463075,-3.9601030984513,0.000964724550051354));
#22123=CARTESIAN_POINT('Origin',(4.7,0.,0.));
#22124=CARTESIAN_POINT('',(-0.155840155369234,-3.95023180461977,0.00295067076493905));
#22125=CARTESIAN_POINT('',(-0.26115984463076,-3.94963863249541,0.00268116949869843));
#22126=CARTESIAN_POINT('',(4.7,-3.954,-4.84225344382863E-16));
#22127=CARTESIAN_POINT('Ctrl Pts',(-0.155840155369234,-3.95023180461977,
0.00295067076493905));
#22128=CARTESIAN_POINT('Ctrl Pts',(-0.16920372862648,-3.95333112739324,
0.446559495418593));
#22129=CARTESIAN_POINT('Ctrl Pts',(-0.182567301883726,-3.88435259221191,
0.889232777547541));
#22130=CARTESIAN_POINT('Ctrl Pts',(-0.195930875140972,-3.73911347548015,
1.30528431062562));
#22131=CARTESIAN_POINT('Ctrl Pts',(-0.235503611794985,-3.30902571319913,
2.53731240940301));
#22132=CARTESIAN_POINT('Ctrl Pts',(-0.275076348448997,-2.21021368105769,
3.53589605582361));
#22133=CARTESIAN_POINT('Ctrl Pts',(-0.314649085103011,-0.94278807937667,
3.84654225915534));
#22134=CARTESIAN_POINT('Ctrl Pts',(-0.354221821757024,0.324637522304346,
4.15718846248707));
#22135=CARTESIAN_POINT('Ctrl Pts',(-0.393794558411038,1.76067669352494,
3.77989722272996));
#22136=CARTESIAN_POINT('Ctrl Pts',(-0.433367295065051,2.71173397427943,
2.88638797926082));
#22137=CARTESIAN_POINT('Ctrl Pts',(-0.472940031719063,3.6627912550339,1.99287873579169));
#22138=CARTESIAN_POINT('Ctrl Pts',(-0.512512768373075,4.12886664532228,
0.583151488610541));
#22139=CARTESIAN_POINT('Ctrl Pts',(-0.552085505027088,3.89783169822067,
-0.701173848933898));
#22140=CARTESIAN_POINT('Ctrl Pts',(-0.5916582416811,3.66679675111907,-1.98549918647834));
#22141=CARTESIAN_POINT('Ctrl Pts',(-0.631230978335113,2.7386514666275,-3.14442261438607));
#22142=CARTESIAN_POINT('Ctrl Pts',(-0.670803714989126,1.53582968661237,
-3.6504744743393));
#22143=CARTESIAN_POINT('Ctrl Pts',(-0.710376451643139,0.333007906597224,
-4.15652633429253));
#22144=CARTESIAN_POINT('Ctrl Pts',(-0.749949188297152,-1.14449036894149,
-4.00970662629123));
#22145=CARTESIAN_POINT('Ctrl Pts',(-0.789521924951166,-2.22420008166029,
-3.27683852376418));
#22146=CARTESIAN_POINT('Ctrl Pts',(-0.828294668423855,-3.2820826355567,
-2.55878591125383));
#22147=CARTESIAN_POINT('Ctrl Pts',(-0.867067411896545,-3.95809726046985,
-1.27814023393776));
#22148=CARTESIAN_POINT('Ctrl Pts',(-0.905840155369234,-3.960321004907,0.000484847720224144));
#22149=CARTESIAN_POINT('Ctrl Pts',(-1.01115984463075,-3.9601030984513,0.000964724550051354));
#22150=CARTESIAN_POINT('Ctrl Pts',(-0.97319709692665,-3.95597340791621,
-1.25113370713065));
#22151=CARTESIAN_POINT('Ctrl Pts',(-0.935234349222548,-3.31169915783721,
-2.50689315478987));
#22152=CARTESIAN_POINT('Ctrl Pts',(-0.897271601518446,-2.29044260664442,
-3.23088376718121));
#22153=CARTESIAN_POINT('Ctrl Pts',(-0.857698864864433,-1.22587486588073,
-3.9855786082252));
#22154=CARTESIAN_POINT('Ctrl Pts',(-0.81812612821042,0.248328626734209,
-4.16244386416014));
#22155=CARTESIAN_POINT('Ctrl Pts',(-0.778553391556407,1.46120239253684,
-3.68098150218274));
#22156=CARTESIAN_POINT('Ctrl Pts',(-0.738980654902394,2.67407615833947,
-3.19951914020535));
#22157=CARTESIAN_POINT('Ctrl Pts',(-0.699407918248381,3.62562019732977,
-2.05972916031563));
#22158=CARTESIAN_POINT('Ctrl Pts',(-0.659835181594368,3.88275101405482,
-0.780372868712951));
#22159=CARTESIAN_POINT('Ctrl Pts',(-0.620262444940355,4.13988183077987,
0.498983422889739));
#22160=CARTESIAN_POINT('Ctrl Pts',(-0.580689708286341,3.70259942523967,
1.9179060262054));
#22161=CARTESIAN_POINT('Ctrl Pts',(-0.541116971632328,2.76992747361883,
2.83058987531903));
#22162=CARTESIAN_POINT('Ctrl Pts',(-0.501544234978315,1.83725552199801,
3.74327372443265));
#22163=CARTESIAN_POINT('Ctrl Pts',(-0.461971498324304,0.409194024296591,
4.14971881934427));
#22164=CARTESIAN_POINT('Ctrl Pts',(-0.422398761670291,-0.864292498870581,
3.8649367042376));
#22165=CARTESIAN_POINT('Ctrl Pts',(-0.382826025016278,-2.13777902203777,
3.58015458913094));
#22166=CARTESIAN_POINT('Ctrl Pts',(-0.343253288362265,-3.25669057067071,
2.60414526400595));
#22167=CARTESIAN_POINT('Ctrl Pts',(-0.303680551708251,-3.71176839821802,
1.3811272965795));
#22168=CARTESIAN_POINT('Ctrl Pts',(-0.289506982682421,-3.87476134604623,
0.943085072391007));
#22169=CARTESIAN_POINT('Ctrl Pts',(-0.27533341365659,-3.95259626783404,
0.473356045129417));
#22170=CARTESIAN_POINT('Ctrl Pts',(-0.26115984463076,-3.94963863249541,
0.00268116949869843));
#22171=CARTESIAN_POINT('Origin',(4.7,0.,0.));
#22172=CARTESIAN_POINT('',(0.594159844630767,-3.95001826622686,-0.00286169934786473));
#22173=CARTESIAN_POINT('',(0.488840155369245,-3.95065042271477,-0.00310251149715996));
#22174=CARTESIAN_POINT('',(4.7,-3.954,-4.84225344382863E-16));
#22175=CARTESIAN_POINT('Ctrl Pts',(0.594159844630767,-3.95001826622686,
-0.00286169934786473));
#22176=CARTESIAN_POINT('Ctrl Pts',(0.568232691297599,-3.94420741043142,
0.857917096057318));
#22177=CARTESIAN_POINT('Ctrl Pts',(0.54230553796443,-3.6674357688023,1.72209758997099));
#22178=CARTESIAN_POINT('Ctrl Pts',(0.516378384631261,-3.14891915370461,
2.40188361031813));
#22179=CARTESIAN_POINT('Ctrl Pts',(0.476805647977248,-2.35750479377407,
3.43944422557712));
#22180=CARTESIAN_POINT('Ctrl Pts',(0.437232911323236,-1.00291986527977,
4.04743834756636));
#22181=CARTESIAN_POINT('Ctrl Pts',(0.397660174669223,0.29831306247853,3.9491449746543));
#22182=CARTESIAN_POINT('Ctrl Pts',(0.35808743801521,1.59954599023685,3.85085160174224));
#22183=CARTESIAN_POINT('Ctrl Pts',(0.318514701361196,2.84742691725918,3.04627073392885));
#22184=CARTESIAN_POINT('Ctrl Pts',(0.278941964707183,3.47399828021787,1.90159739774904));
#22185=CARTESIAN_POINT('Ctrl Pts',(0.23936922805317,4.10056964317655,0.756924061569239));
#22186=CARTESIAN_POINT('Ctrl Pts',(0.199796491399158,4.1058314420716,-0.727841742976961));
#22187=CARTESIAN_POINT('Ctrl Pts',(0.160223754745145,3.48738883424261,-1.87692723164287));
#22188=CARTESIAN_POINT('Ctrl Pts',(0.120651018091132,2.86894622641362,-3.02601272030878));
#22189=CARTESIAN_POINT('Ctrl Pts',(0.0810782814371191,1.62679921186058,
-3.83941789309439));
#22190=CARTESIAN_POINT('Ctrl Pts',(0.0415055447831063,0.326295634599078,
-3.94693145024388));
#22191=CARTESIAN_POINT('Ctrl Pts',(0.00193280812909338,-0.974207942662425,
-4.05444500739337));
#22192=CARTESIAN_POINT('Ctrl Pts',(-0.0376399285249198,-2.33306808263239,
-3.45606694890674));
#22193=CARTESIAN_POINT('Ctrl Pts',(-0.0772126651789329,-3.13181640640708,
-2.42414164409634));
#22194=CARTESIAN_POINT('Ctrl Pts',(-0.1034218285757,-3.66083024524608,-1.7406938663119));
#22195=CARTESIAN_POINT('Ctrl Pts',(-0.129630991972467,-3.94415329137893,
-0.867072334743039));
#22196=CARTESIAN_POINT('Ctrl Pts',(-0.155840155369234,-3.95023180461977,
0.00295067076493905));
#22197=CARTESIAN_POINT('Ctrl Pts',(-0.26115984463076,-3.94963863249541,
0.00268116949869843));
#22198=CARTESIAN_POINT('Ctrl Pts',(-0.235760677002577,-3.94433852243758,
-0.840772588882956));
#22199=CARTESIAN_POINT('Ctrl Pts',(-0.210361509374395,-3.67958948684631,
-1.68726374763685));
#22200=CARTESIAN_POINT('Ctrl Pts',(-0.184962341746213,-3.18051337951411,
-2.35988811050413));
#22201=CARTESIAN_POINT('Ctrl Pts',(-0.1453896050922,-2.40293642680116,-3.40785894043344));
#22202=CARTESIAN_POINT('Ctrl Pts',(-0.105816868438186,-1.05653841491356,
-4.03377399056417));
#22203=CARTESIAN_POINT('Ctrl Pts',(-0.0662441317841735,0.245884260641977,
-3.95275577056508));
#22204=CARTESIAN_POINT('Ctrl Pts',(-0.0266713951301605,1.54830693619751,
-3.87173755056599));
#22205=CARTESIAN_POINT('Ctrl Pts',(0.0129013415238527,2.806754275421,-3.08378606043707));
#22206=CARTESIAN_POINT('Ctrl Pts',(0.0524740781778653,3.44845954321452,
-1.94752767122311));
#22207=CARTESIAN_POINT('Ctrl Pts',(0.0920468148318783,4.09016481100804,
-0.811269282009136));
#22208=CARTESIAN_POINT('Ctrl Pts',(0.131619551485891,4.1151280073716,0.673296006289876));
#22209=CARTESIAN_POINT('Ctrl Pts',(0.171192288139904,3.51198744236147,1.83048667191605));
#22210=CARTESIAN_POINT('Ctrl Pts',(0.210765024793917,2.90884687735135,2.98767733754223));
#22211=CARTESIAN_POINT('Ctrl Pts',(0.250337761447931,1.67760255096752,3.81749338049556));
#22212=CARTESIAN_POINT('Ctrl Pts',(0.289910498101944,0.378640083609367,
3.94225429652265));
#22213=CARTESIAN_POINT('Ctrl Pts',(0.329483234755957,-0.920322383748772,
4.06701521254974));
#22214=CARTESIAN_POINT('Ctrl Pts',(0.369055971409969,-2.28700299208125,
3.48672100165062));
#22215=CARTESIAN_POINT('Ctrl Pts',(0.408628708063982,-3.09937397307536,
2.46548539366795));
#22216=CARTESIAN_POINT('Ctrl Pts',(0.435365857165736,-3.6482489279384,1.77549195304792));
#22217=CARTESIAN_POINT('Ctrl Pts',(0.462103006267491,-3.94408314364839,
0.884210041980504));
#22218=CARTESIAN_POINT('Ctrl Pts',(0.488840155369245,-3.95065042271477,
-0.00310251149715996));
#22219=CARTESIAN_POINT('Origin',(4.7,0.,0.));
#22220=CARTESIAN_POINT('',(1.34415984463077,-3.96026049768271,-0.00065371468560671));
#22221=CARTESIAN_POINT('',(1.23884015536925,-3.9603872214563,-0.000165414599889812));
#22222=CARTESIAN_POINT('',(4.7,-3.954,-4.84225344382863E-16));
#22223=CARTESIAN_POINT('Ctrl Pts',(1.34415984463077,-3.96026049768271,-0.00065371468560671));
#22224=CARTESIAN_POINT('Ctrl Pts',(1.30566911122168,-3.95733483282496,1.26872354929189));
#22225=CARTESIAN_POINT('Ctrl Pts',(1.26717837781259,-3.29247871293452,2.54073655968515));
#22226=CARTESIAN_POINT('Ctrl Pts',(1.2286876444035,-2.24736922314309,3.26099191795255));
#22227=CARTESIAN_POINT('Ctrl Pts',(1.18911490774948,-1.17288092554265,4.00149419192653));
#22228=CARTESIAN_POINT('Ctrl Pts',(1.14954217109547,0.303539635603274,4.15878216827251));
#22229=CARTESIAN_POINT('Ctrl Pts',(1.10996943444146,1.50991791032203,3.66126817075332));
#22230=CARTESIAN_POINT('Ctrl Pts',(1.07039669778744,2.71629618504079,3.16375417323414));
#22231=CARTESIAN_POINT('Ctrl Pts',(1.03082396113343,3.65263217333238,2.01143820184979));
#22232=CARTESIAN_POINT('Ctrl Pts',(0.991251224479416,3.89276413584316,0.7287826128386));
#22233=CARTESIAN_POINT('Ctrl Pts',(0.951678487825403,4.13289609835394,-0.553872976172574));
#22234=CARTESIAN_POINT('Ctrl Pts',(0.912105751171391,3.67682403508393,-1.96686818281059));
#22235=CARTESIAN_POINT('Ctrl Pts',(0.872533014517378,2.73212350244037,-2.86709572241591));
#22236=CARTESIAN_POINT('Ctrl Pts',(0.832960277863366,1.7874229697968,-3.76732326202123));
#22237=CARTESIAN_POINT('Ctrl Pts',(0.793387541209353,0.354093967779691,
-4.15478313459385));
#22238=CARTESIAN_POINT('Ctrl Pts',(0.75381480455534,-0.915501543584075,
-3.85312777335216));
#22239=CARTESIAN_POINT('Ctrl Pts',(0.714242067901327,-2.18509705494786,
-3.55147241211047));
#22240=CARTESIAN_POINT('Ctrl Pts',(0.674669331247314,-3.29095907565829,
-2.56070181705443));
#22241=CARTESIAN_POINT('Ctrl Pts',(0.635096594593301,-3.72976819033012,
-1.33175296526204));
#22242=CARTESIAN_POINT('Ctrl Pts',(0.621451011272456,-3.8810795941522,-0.907983335660524));
#22243=CARTESIAN_POINT('Ctrl Pts',(0.607805427951612,-3.95307654709183,
-0.455893647073924));
#22244=CARTESIAN_POINT('Ctrl Pts',(0.594159844630767,-3.95001826622686,
-0.00286169934786473));
#22245=CARTESIAN_POINT('Ctrl Pts',(0.488840155369245,-3.95065042271477,
-0.00310251149715996));
#22246=CARTESIAN_POINT('Ctrl Pts',(0.501675742921504,-3.95380314797787,
-0.429070812120259));
#22247=CARTESIAN_POINT('Ctrl Pts',(0.514511330473762,-3.89029053186911,
-0.854124322474488));
#22248=CARTESIAN_POINT('Ctrl Pts',(0.527346918026021,-3.75610460203848,
-1.2555538498656));
#22249=CARTESIAN_POINT('Ctrl Pts',(0.566919654680034,-3.34240289635171,
-2.49318048035031));
#22250=CARTESIAN_POINT('Ctrl Pts',(0.606492391334046,-2.25693813132239,
-3.5062567362535));
#22251=CARTESIAN_POINT('Ctrl Pts',(0.646065127988059,-0.993746163797144,
-3.83369349496089));
#22252=CARTESIAN_POINT('Ctrl Pts',(0.685637864642072,0.26944580372809,-4.16113025366827));
#22253=CARTESIAN_POINT('Ctrl Pts',(0.725210601296086,1.71036497374923,-3.80292751517983));
#22254=CARTESIAN_POINT('Ctrl Pts',(0.764783337950099,2.67319481518899,-2.9221168237108));
#22255=CARTESIAN_POINT('Ctrl Pts',(0.804356074604112,3.63602465662875,-2.04130613224176));
#22256=CARTESIAN_POINT('Ctrl Pts',(0.843928811258124,4.12076516948713,-0.637887487792129));
#22257=CARTESIAN_POINT('Ctrl Pts',(0.883501547912137,3.9067927072547,0.649390478763368));
#22258=CARTESIAN_POINT('Ctrl Pts',(0.92307428456615,3.69282024502226,1.93666844531887));
#22259=CARTESIAN_POINT('Ctrl Pts',(0.962647021220164,2.78013480769901,3.10780573398024));
#22260=CARTESIAN_POINT('Ctrl Pts',(1.00221975787418,1.58413387900453,3.62977369883537));
#22261=CARTESIAN_POINT('Ctrl Pts',(1.04179249452819,0.388132950310035,4.15174166369052));
#22262=CARTESIAN_POINT('Ctrl Pts',(1.0813652311822,-1.09118346975568,4.02454030473942));
#22263=CARTESIAN_POINT('Ctrl Pts',(1.12093796783622,-2.18052281686445,3.30606374658756));
#22264=CARTESIAN_POINT('Ctrl Pts',(1.16023869701389,-3.26237447240231,2.59252571460078));
#22265=CARTESIAN_POINT('Ctrl Pts',(1.19953942619157,-3.95959172893657,1.29581293552976));
#22266=CARTESIAN_POINT('Ctrl Pts',(1.23884015536925,-3.9603872214563,-0.000165414599889812));
#22267=CARTESIAN_POINT('Origin',(4.7,0.,0.));
#22268=CARTESIAN_POINT('',(2.09415984463077,-3.95182140471939,0.00339740089000562));
#22269=CARTESIAN_POINT('',(1.98884015536925,-3.95110529642541,0.00323787354723457));
#22270=CARTESIAN_POINT('',(4.7,-3.954,-4.84225344382863E-16));
#22271=CARTESIAN_POINT('Ctrl Pts',(2.09415984463077,-3.95182140471939,0.00339740089000562));
#22272=CARTESIAN_POINT('Ctrl Pts',(2.08267826779977,-3.95497662709706,0.384145209727677));
#22273=CARTESIAN_POINT('Ctrl Pts',(2.07119669096877,-3.90439221631175,0.764072168098434));
#22274=CARTESIAN_POINT('Ctrl Pts',(2.05971511413777,-3.79664813820596,1.12703133440906));
#22275=CARTESIAN_POINT('Ctrl Pts',(2.02014237748376,-3.42529426480786,2.37801695389204));
#22276=CARTESIAN_POINT('Ctrl Pts',(1.98056964082974,-2.37492629601307,3.42743789470054));
#22277=CARTESIAN_POINT('Ctrl Pts',(1.94099690417573,-1.12360621613093,3.79766320059515));
#22278=CARTESIAN_POINT('Ctrl Pts',(1.90142416752171,0.127713863751167,4.16788850648974));
#22279=CARTESIAN_POINT('Ctrl Pts',(1.8618514308677,1.57998605472057,3.85891817747047));
#22280=CARTESIAN_POINT('Ctrl Pts',(1.82227869421369,2.57222663869159,3.011376235758));
#22281=CARTESIAN_POINT('Ctrl Pts',(1.78270595755968,3.56446722266259,2.16383429404553));
#22282=CARTESIAN_POINT('Ctrl Pts',(1.74313322090566,4.0966761996352,0.777720739639841));
#22283=CARTESIAN_POINT('Ctrl Pts',(1.70356048425165,3.9266252390076,-0.516091994193958));
#22284=CARTESIAN_POINT('Ctrl Pts',(1.66398774759764,3.75657427838,-1.80990472802779));
#22285=CARTESIAN_POINT('Ctrl Pts',(1.62441501094363,2.88426338015217,-3.01141664128973));
#22286=CARTESIAN_POINT('Ctrl Pts',(1.58484227428961,1.70671405614722,-3.57377445352));
#22287=CARTESIAN_POINT('Ctrl Pts',(1.5452695376356,0.52916473214227,-4.13613226575025));
#22288=CARTESIAN_POINT('Ctrl Pts',(1.50569680098158,-0.953623017639813,
-4.05933597694883));
#22289=CARTESIAN_POINT('Ctrl Pts',(1.46612406432757,-2.06677669610277,-3.37833846772776));
#22290=CARTESIAN_POINT('Ctrl Pts',(1.42655132767356,-3.17993037456572,-2.6973409585067));
#22291=CARTESIAN_POINT('Ctrl Pts',(1.38697859101955,-3.92344998170957,-1.41214222886602));
#22292=CARTESIAN_POINT('Ctrl Pts',(1.34740585436553,-3.95893176825402,-0.107684578244696));
#22293=CARTESIAN_POINT('Ctrl Pts',(1.34632385112061,-3.9599019161746,-0.0720179165433403));
#22294=CARTESIAN_POINT('Ctrl Pts',(1.34524184787569,-3.96034274030552,-0.036336857016415));
#22295=CARTESIAN_POINT('Ctrl Pts',(1.34415984463077,-3.96026049768271,-0.00065371468560671));
#22296=CARTESIAN_POINT('Ctrl Pts',(1.23884015536925,-3.9603872214563,-0.000165414599889812));
#22297=CARTESIAN_POINT('Ctrl Pts',(1.23911216284558,-3.96039272720434,-0.00913511586959148));
#22298=CARTESIAN_POINT('Ctrl Pts',(1.23938417032192,-3.96036487243322,-0.0181047819581257));
#22299=CARTESIAN_POINT('Ctrl Pts',(1.23965617779825,-3.96030355377182,-0.0270742192741198));
#22300=CARTESIAN_POINT('Ctrl Pts',(1.27922891445227,-3.95138266941864,-1.33198386963134));
#22301=CARTESIAN_POINT('Ctrl Pts',(1.31880165110628,-3.23417862656048,-2.63205141299318));
#22302=CARTESIAN_POINT('Ctrl Pts',(1.35837438776029,-2.13511797100763,-3.33556719333418));
#22303=CARTESIAN_POINT('Ctrl Pts',(1.3979471244143,-1.03605731545477,-4.03908297367518));
#22304=CARTESIAN_POINT('Ctrl Pts',(1.43751986106832,0.444859952792789,-4.14604699099532));
#22305=CARTESIAN_POINT('Ctrl Pts',(1.47709259772233,1.63361266316492,-3.60777589632646));
#22306=CARTESIAN_POINT('Ctrl Pts',(1.51666533437635,2.82236537353706,-3.06950480165761));
#22307=CARTESIAN_POINT('Ctrl Pts',(1.55623807103036,3.71895352603377,-1.88599859499978));
#22308=CARTESIAN_POINT('Ctrl Pts',(1.59581080768437,3.91530611694513,-0.595915482244824));
#22309=CARTESIAN_POINT('Ctrl Pts',(1.63538354433838,4.11165870785648,0.694167630510099));
#22310=CARTESIAN_POINT('Ctrl Pts',(1.6749562809924,3.60777573718251,2.09082764936215));
#22311=CARTESIAN_POINT('Ctrl Pts',(1.71452901764641,2.63299330424895,2.95839204824972));
#22312=CARTESIAN_POINT('Ctrl Pts',(1.75410175430042,1.65821087131538,3.82595644713731));
#22313=CARTESIAN_POINT('Ctrl Pts',(1.79367449095443,0.212528976122227,4.16442522606043));
#22314=CARTESIAN_POINT('Ctrl Pts',(1.83324722760845,-1.0460681548226,3.81974850832264));
#22315=CARTESIAN_POINT('Ctrl Pts',(1.87281996426246,-2.30466528576745,3.47507179058484));
#22316=CARTESIAN_POINT('Ctrl Pts',(1.91239270091647,-3.37617765246396,2.44724957618611));
#22317=CARTESIAN_POINT('Ctrl Pts',(1.95196543757049,-3.77291965952719,1.20408242829145));
#22318=CARTESIAN_POINT('Ctrl Pts',(1.96425701017007,-3.89615054006395,0.81794589734172));
#22319=CARTESIAN_POINT('Ctrl Pts',(1.97654858276966,-3.95428175936265,0.41103358390573));
#22320=CARTESIAN_POINT('Ctrl Pts',(1.98884015536925,-3.95110529642541,0.00323787354723457));
#22321=CARTESIAN_POINT('Origin',(4.7,0.,0.));
#22322=CARTESIAN_POINT('',(2.84415984463077,-3.94879606319858,-0.00214324138103211));
#22323=CARTESIAN_POINT('',(2.73884015536925,-3.94927650700756,-0.0024772734444678));
#22324=CARTESIAN_POINT('',(4.7,-3.954,-4.84225344382863E-16));
#22325=CARTESIAN_POINT('Ctrl Pts',(2.84415984463077,-3.94879606319858,-0.00214324138103211));
#22326=CARTESIAN_POINT('Ctrl Pts',(2.82011468772384,-3.94483830299845,0.796774452968311));
#22327=CARTESIAN_POINT('Ctrl Pts',(2.79606953081692,-3.70949558657619,1.5978361366702));
#22328=CARTESIAN_POINT('Ctrl Pts',(2.77202437391,-3.25896341504729,2.25030979499844));
#22329=CARTESIAN_POINT('Ctrl Pts',(2.73245163725599,-2.51749223034729,3.3241297062035));
#22330=CARTESIAN_POINT('Ctrl Pts',(2.69287890060197,-1.19316953698868,3.99549144530754));
#22331=CARTESIAN_POINT('Ctrl Pts',(2.65330616394796,0.111255577602164,3.95883302382597));
#22332=CARTESIAN_POINT('Ctrl Pts',(2.61373342729395,1.41568069219301,3.9221746023444));
#22333=CARTESIAN_POINT('Ctrl Pts',(2.57416069063994,2.70020822801613,3.17749602027721));
#22334=CARTESIAN_POINT('Ctrl Pts',(2.53458795398592,3.38020137119358,2.06372852000055));
#22335=CARTESIAN_POINT('Ctrl Pts',(2.49501521733191,4.06019451437106,0.949961019723846));
#22336=CARTESIAN_POINT('Ctrl Pts',(2.4554424806779,4.13565326490285,-0.532895398762326));
#22337=CARTESIAN_POINT('Ctrl Pts',(2.41586974402388,3.57223350617034,-1.70993698465078));
#22338=CARTESIAN_POINT('Ctrl Pts',(2.37629700736987,3.00881374743785,-2.88697857053918));
#22339=CARTESIAN_POINT('Ctrl Pts',(2.33672427071586,1.80651547944111,-3.75820532382986));
#22340=CARTESIAN_POINT('Ctrl Pts',(2.29715153406185,0.512549882267534,-3.92708916785323));
#22341=CARTESIAN_POINT('Ctrl Pts',(2.25757879740783,-0.78141571490604,-4.09597301187659));
#22342=CARTESIAN_POINT('Ctrl Pts',(2.21800606075382,-2.16704864125646,-3.56251394663264));
#22343=CARTESIAN_POINT('Ctrl Pts',(2.17843332409981,-3.01369521543096,-2.56950926493196));
#22344=CARTESIAN_POINT('Ctrl Pts',(2.15034216427679,-3.6146969716825,-1.86461353172711));
#22345=CARTESIAN_POINT('Ctrl Pts',(2.12225100445378,-3.94410174587872,-0.928151262481906));
#22346=CARTESIAN_POINT('Ctrl Pts',(2.09415984463077,-3.95182140471939,0.00339740089000562));
#22347=CARTESIAN_POINT('Ctrl Pts',(1.98884015536925,-3.95110529642541,0.00323787354723457));
#22348=CARTESIAN_POINT('Ctrl Pts',(2.01612131942367,-3.94405513211149,-0.901865324993545));
#22349=CARTESIAN_POINT('Ctrl Pts',(2.0434024834781,-3.63499186103326,-1.81132030196311));
#22350=CARTESIAN_POINT('Ctrl Pts',(2.07068364753253,-3.06537576631618,-2.50763008887844));
#22351=CARTESIAN_POINT('Ctrl Pts',(2.11025638418654,-2.23911821861202,-3.51766337676301));
#22352=CARTESIAN_POINT('Ctrl Pts',(2.14982912084055,-0.86463147577378,-4.07921787114163));
#22353=CARTESIAN_POINT('Ctrl Pts',(2.18940185749456,0.432503828354505,-3.93670899227079));
#22354=CARTESIAN_POINT('Ctrl Pts',(2.22897459414858,1.72963913248281,-3.79420011339995));
#22355=CARTESIAN_POINT('Ctrl Pts',(2.26854733080259,2.94942299790115,-2.94762786127962));
#22356=CARTESIAN_POINT('Ctrl Pts',(2.3081200674566,3.53668589121304,-1.78229912143322));
#22357=CARTESIAN_POINT('Ctrl Pts',(2.34769280411062,4.12394878452495,-0.616970381586784));
#22358=CARTESIAN_POINT('Ctrl Pts',(2.38726554076463,4.07869070573037,0.867114845985733));
#22359=CARTESIAN_POINT('Ctrl Pts',(2.42683827741864,3.42151030939356,1.99449353322607));
#22360=CARTESIAN_POINT('Ctrl Pts',(2.46641101407266,2.76432991305676,3.12187222046637));
#22361=CARTESIAN_POINT('Ctrl Pts',(2.50598375072667,1.49522719917778,3.89254436737451));
#22362=CARTESIAN_POINT('Ctrl Pts',(2.54555648738068,0.191818564785084,3.95574808216736));
#22363=CARTESIAN_POINT('Ctrl Pts',(2.5851292240347,-1.11159006960763,4.01895179696022));
#22364=CARTESIAN_POINT('Ctrl Pts',(2.62470196068871,-2.44930462451406,3.37468707963778));
#22365=CARTESIAN_POINT('Ctrl Pts',(2.66427469734272,-3.21248087242804,2.31618304450469));
#22366=CARTESIAN_POINT('Ctrl Pts',(2.68912985001823,-3.69182255470969,1.65134958527496));
#22367=CARTESIAN_POINT('Ctrl Pts',(2.71398500269374,-3.94451216648441,0.823101088397621));
#22368=CARTESIAN_POINT('Ctrl Pts',(2.73884015536925,-3.94927650700756,-0.0024772734444678));
#22369=CARTESIAN_POINT('Origin',(4.7,0.,0.));
#22370=CARTESIAN_POINT('',(3.59415984463077,-3.95946408857375,-0.00171547380415804));
#22371=CARTESIAN_POINT('',(3.48884015536925,-3.95988464442629,-0.0012757644514219));
#22372=CARTESIAN_POINT('',(4.7,-3.954,-4.84225344382863E-16));
#22373=CARTESIAN_POINT('Ctrl Pts',(3.59415984463077,-3.95946408857375,-0.00171547380415804));
#22374=CARTESIAN_POINT('Ctrl Pts',(3.55755110764792,-3.95286445098715,1.20624346856487));
#22375=CARTESIAN_POINT('Ctrl Pts',(3.52094237066508,-3.35954953332255,2.41981313494161));
#22376=CARTESIAN_POINT('Ctrl Pts',(3.48433363368223,-2.39904223913318,3.15108442427959));
#22377=CARTESIAN_POINT('Ctrl Pts',(3.44476089702822,-1.36076817288979,3.94156255984524));
#22378=CARTESIAN_POINT('Ctrl Pts',(3.4051881603742,0.106564219678576,4.16848287757163));
#22379=CARTESIAN_POINT('Ctrl Pts',(3.36561542372019,1.33511675607524,3.72856540263541));
#22380=CARTESIAN_POINT('Ctrl Pts',(3.32604268706618,2.56366929247188,3.2886479276992));
#22381=CARTESIAN_POINT('Ctrl Pts',(3.28646995041217,3.55344197269683,2.1818926601004));
#22382=CARTESIAN_POINT('Ctrl Pts',(3.24689721375816,3.85395200825982,0.912025565492931));
#22383=CARTESIAN_POINT('Ctrl Pts',(3.20732447710414,4.15446204382282,-0.357841529114534));
#22384=CARTESIAN_POINT('Ctrl Pts',(3.16775174045013,3.76570943472387,-1.79082045073066));
#22385=CARTESIAN_POINT('Ctrl Pts',(3.12817900379612,2.86463012077892,-2.73470857409136));
#22386=CARTESIAN_POINT('Ctrl Pts',(3.0886062671421,1.96355080683398,-3.67859669745204));
#22387=CARTESIAN_POINT('Ctrl Pts',(3.04903353048809,0.550144788043063,-4.13339402255731));
#22388=CARTESIAN_POINT('Ctrl Pts',(3.00946079383408,-0.732293674866088,
-3.89210517430269));
#22389=CARTESIAN_POINT('Ctrl Pts',(2.96988805718007,-2.01473213777531,-3.65081632604805));
#22390=CARTESIAN_POINT('Ctrl Pts',(2.93031532052605,-3.16620304480276,-2.71344130443343));
#22391=CARTESIAN_POINT('Ctrl Pts',(2.89074258387204,-3.66262866029575,-1.50661475197305));
#22392=CARTESIAN_POINT('Ctrl Pts',(2.87521500412495,-3.85741651134733,-1.03307925459082));
#22393=CARTESIAN_POINT('Ctrl Pts',(2.85968742437786,-3.95135185592497,-0.518058286493471));
#22394=CARTESIAN_POINT('Ctrl Pts',(2.84415984463077,-3.94879606319858,-0.00214324138103211));
#22395=CARTESIAN_POINT('Ctrl Pts',(2.73884015536925,-3.94927650700756,-0.0024772734444678));
#22396=CARTESIAN_POINT('Ctrl Pts',(2.75355773934775,-3.95209763559475,-0.49133039093987));
#22397=CARTESIAN_POINT('Ctrl Pts',(2.76827532332625,-3.86799050714696,-0.979247298167196));
#22398=CARTESIAN_POINT('Ctrl Pts',(2.78299290730476,-3.69253847048653,-1.43174610016721));
#22399=CARTESIAN_POINT('Ctrl Pts',(2.82256564395877,-3.2207818797095,-2.6484278567624));
#22400=CARTESIAN_POINT('Ctrl Pts',(2.86213838061279,-2.08863075723384,-3.60904801700904));
#22401=CARTESIAN_POINT('Ctrl Pts',(2.9017111172668,-0.811369677826096,-3.87639220116739));
#22402=CARTESIAN_POINT('Ctrl Pts',(2.94128385392081,0.465891401581615,-4.14373638532573));
#22403=CARTESIAN_POINT('Ctrl Pts',(2.98085659057482,1.88826243792143,-3.71780459339582));
#22404=CARTESIAN_POINT('Ctrl Pts',(3.02042932722884,2.80836885365649,-2.79245441022394));
#22405=CARTESIAN_POINT('Ctrl Pts',(3.06000206388285,3.72847526939156,-1.86710422705205));
#22406=CARTESIAN_POINT('Ctrl Pts',(3.09957480053686,4.14631706452186,-0.442335652638224));
#22407=CARTESIAN_POINT('Ctrl Pts',(3.13914753719087,3.87171871614322,0.833385525692216));
#22408=CARTESIAN_POINT('Ctrl Pts',(3.17872027384489,3.59712036776459,2.10910670402262));
#22409=CARTESIAN_POINT('Ctrl Pts',(3.2182930104989,2.63008187587697,3.23578048626965));
#22410=CARTESIAN_POINT('Ctrl Pts',(3.25786574715291,1.41073884444955,3.70061524129814));
#22411=CARTESIAN_POINT('Ctrl Pts',(3.29743848380693,0.191395813022067,4.16544999632666));
#22412=CARTESIAN_POINT('Ctrl Pts',(3.33701122046094,-1.28025175794523,3.96844572413664));
#22413=CARTESIAN_POINT('Ctrl Pts',(3.37658395711496,-2.33440168590114,3.19926648159057));
#22414=CARTESIAN_POINT('Ctrl Pts',(3.41400268986639,-3.33117263907,2.47195482845881));
#22415=CARTESIAN_POINT('Ctrl Pts',(3.45142142261782,-3.95465904777607,1.23306166885008));
#22416=CARTESIAN_POINT('Ctrl Pts',(3.48884015536925,-3.95988464442629,-0.0012757644514219));
#22417=CARTESIAN_POINT('Origin',(4.7,0.,0.));
#22418=CARTESIAN_POINT('',(4.34415984463077,-3.95361637884632,0.00355905447742291));
#22419=CARTESIAN_POINT('',(4.23884015536925,-3.95282662999892,0.00352652566842014));
#22420=CARTESIAN_POINT('',(4.7,-3.954,-4.84225344382863E-16));
#22421=CARTESIAN_POINT('Ctrl Pts',(4.34415984463077,-3.95361637884632,0.00355905447742291));
#22422=CARTESIAN_POINT('Ctrl Pts',(4.33456026422602,-3.9564854253942,0.321529051071549));
#22423=CARTESIAN_POINT('Ctrl Pts',(4.32496068382126,-3.92132433711414,0.638872526236415));
#22424=CARTESIAN_POINT('Ctrl Pts',(4.3153611034165,-3.84569027880081,0.946257361197047));
#22425=CARTESIAN_POINT('Ctrl Pts',(4.27578836676249,-3.53390095619407,2.21340223758226));
#22426=CARTESIAN_POINT('Ctrl Pts',(4.23621563010848,-2.53432656349926,3.31131307838228));
#22427=CARTESIAN_POINT('Ctrl Pts',(4.19664289345447,-1.3019110173562,3.74028934936446));
#22428=CARTESIAN_POINT('Ctrl Pts',(4.15707015680045,-0.0694954712131363,
4.16926562034663));
#22429=CARTESIAN_POINT('Ctrl Pts',(4.11749742014644,1.39576122837819,3.92930732151097));
#22430=CARTESIAN_POINT('Ctrl Pts',(4.07792468349243,2.42696562489611,3.12962850345776));
#22431=CARTESIAN_POINT('Ctrl Pts',(4.03835194683841,3.45817002141404,2.32994968540454));
#22432=CARTESIAN_POINT('Ctrl Pts',(3.99877921018441,4.05532211485856,0.970550348133779));
#22433=CARTESIAN_POINT('Ctrl Pts',(3.95920647353039,3.94663551873683,-0.329855720471081));
#22434=CARTESIAN_POINT('Ctrl Pts',(3.91963373687638,3.8379489226151,-1.63026178907598));
#22435=CARTESIAN_POINT('Ctrl Pts',(3.88006100022236,3.02342363692707,-2.87167458901497));
#22436=CARTESIAN_POINT('Ctrl Pts',(3.84048826356835,1.87378076695643,-3.48908044496925));
#22437=CARTESIAN_POINT('Ctrl Pts',(3.80091552691433,0.724137896985802,-4.10648630092352));
#22438=CARTESIAN_POINT('Ctrl Pts',(3.76134279026032,-0.760622557267377,
-4.09988521289311));
#22439=CARTESIAN_POINT('Ctrl Pts',(3.72177005360631,-1.90473024667613,-3.47228158441675));
#22440=CARTESIAN_POINT('Ctrl Pts',(3.6821973169523,-3.04883793608485,-2.84467795594042));
#22441=CARTESIAN_POINT('Ctrl Pts',(3.64262458029828,-3.85229286064914,-1.5960717870181));
#22442=CARTESIAN_POINT('Ctrl Pts',(3.60305184364427,-3.94941245297207,-0.294750725854538));
#22443=CARTESIAN_POINT('Ctrl Pts',(3.6000878439731,-3.95668671459885,-0.197281722608817));
#22444=CARTESIAN_POINT('Ctrl Pts',(3.59712384430194,-3.95999842341425,-0.0995169879520828));
#22445=CARTESIAN_POINT('Ctrl Pts',(3.59415984463077,-3.95946408857375,-0.00171547380415804));
#22446=CARTESIAN_POINT('Ctrl Pts',(3.48884015536925,-3.95988464442629,-0.0012757644514219));
#22447=CARTESIAN_POINT('Ctrl Pts',(3.49099415927183,-3.9601854551366,-0.0723302190770247));
#22448=CARTESIAN_POINT('Ctrl Pts',(3.49314816317441,-3.95843752728934,-0.143369577335591));
#22449=CARTESIAN_POINT('Ctrl Pts',(3.49530216707699,-3.95459413083459,-0.214295384307806));
#22450=CARTESIAN_POINT('Ctrl Pts',(3.534874903731,-3.8839843628677,-1.51732379475814));
#22451=CARTESIAN_POINT('Ctrl Pts',(3.57444764038502,-3.10611254198946,-2.78202640275678));
#22452=CARTESIAN_POINT('Ctrl Pts',(3.61402037703903,-1.97501740250559,-3.43278946502215));
#22453=CARTESIAN_POINT('Ctrl Pts',(3.65359311369304,-0.843922263021716,
-4.08355252728753));
#22454=CARTESIAN_POINT('Ctrl Pts',(3.69316585034705,0.640396195067791,-4.12037604381963));
#22455=CARTESIAN_POINT('Ctrl Pts',(3.73273858700107,1.80236879172075,-3.52650024670325));
#22456=CARTESIAN_POINT('Ctrl Pts',(3.77231132365508,2.96434138837375,-2.93262444958684));
#22457=CARTESIAN_POINT('Ctrl Pts',(3.8118840603091,3.80396812359018,-1.70804933882191));
#22458=CARTESIAN_POINT('Ctrl Pts',(3.85145679696311,3.93910327792533,-0.410125123840174));
#22459=CARTESIAN_POINT('Ctrl Pts',(3.89102953361713,4.07423843226048,0.887799091141527));
#22460=CARTESIAN_POINT('Ctrl Pts',(3.93060227027114,3.50488200571439,2.25907241034003));
#22461=CARTESIAN_POINT('Ctrl Pts',(3.97017500692515,2.49016953091971,3.07957674991972));
#22462=CARTESIAN_POINT('Ctrl Pts',(4.00974774357916,1.47545705612503,3.90008108949941));
#22463=CARTESIAN_POINT('Ctrl Pts',(4.04932048023317,0.0153885330817553,
4.16981644946029));
#22464=CARTESIAN_POINT('Ctrl Pts',(4.08889321688719,-1.22550391604859,3.76601611827626));
#22465=CARTESIAN_POINT('Ctrl Pts',(4.1284659535412,-2.46639636517894,3.36221578709222));
#22466=CARTESIAN_POINT('Ctrl Pts',(4.16803869019521,-3.48811274039636,2.28487976476326));
#22467=CARTESIAN_POINT('Ctrl Pts',(4.20761142684922,-3.82563147568885,1.02434421147664));
#22468=CARTESIAN_POINT('Ctrl Pts',(4.21802100302256,-3.91441550434159,0.69276135998306));
#22469=CARTESIAN_POINT('Ctrl Pts',(4.22843057919591,-3.95585656325474,0.348502039960021));
#22470=CARTESIAN_POINT('Ctrl Pts',(4.23884015536925,-3.95282662999892,0.00352652566842014));
#22471=CARTESIAN_POINT('Origin',(4.7,0.,0.));
#22472=CARTESIAN_POINT('',(5.09415984463078,-3.94797828517504,-0.00125412662908497));
#22473=CARTESIAN_POINT('',(4.98884015536925,-3.94827688052699,-0.00165327621010028));
#22474=CARTESIAN_POINT('',(4.7,-3.954,-4.84225344382863E-16));
#22475=CARTESIAN_POINT('Ctrl Pts',(5.09415984463078,-3.94797828517504,-0.00125412662908497));
#22476=CARTESIAN_POINT('Ctrl Pts',(5.0719966841501,-3.94586967481992,0.735514823501616));
#22477=CARTESIAN_POINT('Ctrl Pts',(5.04983352366942,-3.74808709220802,1.47333516746832));
#22478=CARTESIAN_POINT('Ctrl Pts',(5.02767036318874,-3.36171787287947,2.09370238029319));
#22479=CARTESIAN_POINT('Ctrl Pts',(4.98809762653473,-2.67184842122634,3.20137961627701));
#22480=CARTESIAN_POINT('Ctrl Pts',(4.94852488988071,-1.38075027064227,3.93460723880349));
#22481=CARTESIAN_POINT('Ctrl Pts',(4.9089521532267,-0.0760507690123915,
3.95966576804347));
#22482=CARTESIAN_POINT('Ctrl Pts',(4.86937941657269,1.22864873261751,3.98472429728344));
#22483=CARTESIAN_POINT('Ctrl Pts',(4.82980667991868,2.54694958529321,3.30161373323687));
#22484=CARTESIAN_POINT('Ctrl Pts',(4.79023394326466,3.27884346786418,2.22124339668733));
#22485=CARTESIAN_POINT('Ctrl Pts',(4.75066120661065,4.01073735043511,1.14087306013782));
#22486=CARTESIAN_POINT('Ctrl Pts',(4.71108846995663,4.15622426290134,-0.336757048914672));
#22487=CARTESIAN_POINT('Ctrl Pts',(4.67151573330262,3.64908763723056,-1.53912186973409));
#22488=CARTESIAN_POINT('Ctrl Pts',(4.63194299664861,3.14195101155977,-2.74148669055352));
#22489=CARTESIAN_POINT('Ctrl Pts',(4.5923702599946,1.98219084775198,-3.66858622313989));
#22490=CARTESIAN_POINT('Ctrl Pts',(4.55279752334059,0.697657634116575,-3.89846258666689));
#22491=CARTESIAN_POINT('Ctrl Pts',(4.51322478668657,-0.586875579518827,
-4.12833895019389));
#22492=CARTESIAN_POINT('Ctrl Pts',(4.47365205003256,-1.99618184298182,-3.6609921446615));
#22493=CARTESIAN_POINT('Ctrl Pts',(4.43407931337854,-2.888832848454,-2.7091292859101));
#22494=CARTESIAN_POINT('Ctrl Pts',(4.40410615712929,-3.56494398772144,-1.9881699435562));
#22495=CARTESIAN_POINT('Ctrl Pts',(4.37413300088003,-3.94465823934023,-0.989251463133344));
#22496=CARTESIAN_POINT('Ctrl Pts',(4.34415984463077,-3.95361637884632,0.00355905447742291));
#22497=CARTESIAN_POINT('Ctrl Pts',(4.23884015536925,-3.95282662999892,0.00352652566842014));
#22498=CARTESIAN_POINT('Ctrl Pts',(4.26800331584992,-3.94433805867635,-0.962946663792761));
#22499=CARTESIAN_POINT('Ctrl Pts',(4.29716647633059,-3.58680571057285,-1.93504111646879));
#22500=CARTESIAN_POINT('Ctrl Pts',(4.32632963681127,-2.94338137561686,-2.64976288166296));
#22501=CARTESIAN_POINT('Ctrl Pts',(4.36590237346528,-2.07029144488486,-3.61959933727155));
#22502=CARTESIAN_POINT('Ctrl Pts',(4.40547511011929,-0.67079048805332,-4.11553716424445));
#22503=CARTESIAN_POINT('Ctrl Pts',(4.4450478467733,0.618155951047059,-3.91185639710254));
#22504=CARTESIAN_POINT('Ctrl Pts',(4.48462058342732,1.90710239014744,-3.70817562996064));
#22505=CARTESIAN_POINT('Ctrl Pts',(4.52419332008133,3.08549431151664,-2.80487626870394));
#22506=CARTESIAN_POINT('Ctrl Pts',(4.56376605673534,3.61700121293053,-1.61308384066856));
#22507=CARTESIAN_POINT('Ctrl Pts',(4.60333879338935,4.14850811434442,-0.421291412633197));
#22508=CARTESIAN_POINT('Ctrl Pts',(4.64291153004337,4.033129995803,1.05899408218087));
#22509=CARTESIAN_POINT('Ctrl Pts',(4.68248426669738,3.32337978033369,2.15403901706449));
#22510=CARTESIAN_POINT('Ctrl Pts',(4.7220570033514,2.61362956486436,3.24908395194817));
#22511=CARTESIAN_POINT('Ctrl Pts',(4.76162974000541,1.3095072524671,3.95888832690141));
#22512=CARTESIAN_POINT('Ctrl Pts',(4.80120247665942,0.00456797712235453,
3.96039346340133));
#22513=CARTESIAN_POINT('Ctrl Pts',(4.84077521331344,-1.30037129822235,3.96189859990126));
#22514=CARTESIAN_POINT('Ctrl Pts',(4.88034794996745,-2.60612753651453,3.25510449794791));
#22515=CARTESIAN_POINT('Ctrl Pts',(4.91992068662146,-3.31840194262003,2.16169974755576));
#22516=CARTESIAN_POINT('Ctrl Pts',(4.94289384287072,-3.73189852151165,1.52694561381809));
#22517=CARTESIAN_POINT('Ctrl Pts',(4.96586699911999,-3.9453828521266,0.761897912850191));
#22518=CARTESIAN_POINT('Ctrl Pts',(4.98884015536925,-3.94827688052699,-0.00165327621010028));
#22519=CARTESIAN_POINT('Origin',(4.7,0.,0.));
#22520=CARTESIAN_POINT('',(5.84415984463077,-3.95812868148667,-0.00259109635525723));
#22521=CARTESIAN_POINT('',(5.73884015536925,-3.95875693366943,-0.00224257783873754));
#22522=CARTESIAN_POINT('',(4.7,-3.954,-4.84225344382863E-16));
#22523=CARTESIAN_POINT('Ctrl Pts',(5.84415984463077,-3.95812868148667,-0.00259109635525723));
#22524=CARTESIAN_POINT('Ctrl Pts',(5.80943310407417,-3.94941271527673,1.14428747213603));
#22525=CARTESIAN_POINT('Ctrl Pts',(5.77470636351757,-3.4226605516743,2.29814636133711));
#22526=CARTESIAN_POINT('Ctrl Pts',(5.73997962296097,-2.54534896397193,3.03412843592516));
#22527=CARTESIAN_POINT('Ctrl Pts',(5.70040688630696,-1.54561158962567,3.87281425420047));
#22528=CARTESIAN_POINT('Ctrl Pts',(5.66083414965294,-0.0906495641330535,
4.16885932720762));
#22529=CARTESIAN_POINT('Ctrl Pts',(5.62126141299893,1.15732914951951,3.78752240306972));
#22530=CARTESIAN_POINT('Ctrl Pts',(5.58168867634492,2.40530786317208,3.40618547893183));
#22531=CARTESIAN_POINT('Ctrl Pts',(5.54211593969091,3.44630326498462,2.34746655764887));
#22532=CARTESIAN_POINT('Ctrl Pts',(5.5025432030369,3.80651917853864,1.09322845622502));
#22533=CARTESIAN_POINT('Ctrl Pts',(5.46297046638288,4.16673509209267,-0.161009645198846));
#22534=CARTESIAN_POINT('Ctrl Pts',(5.42339772972887,3.84617151738819,-1.61076692676359));
#22535=CARTESIAN_POINT('Ctrl Pts',(5.38382499307485,2.99072899897088,-2.59620430028094));
#22536=CARTESIAN_POINT('Ctrl Pts',(5.34425225642084,2.13528648055357,-3.58164167379831));
#22537=CARTESIAN_POINT('Ctrl Pts',(5.30467951976683,0.744965018423408,-4.10275913926823));
#22538=CARTESIAN_POINT('Ctrl Pts',(5.26510678311281,-0.547447777020062,
-3.92237653030894));
#22539=CARTESIAN_POINT('Ctrl Pts',(5.2255340464588,-1.8398605724635,-3.74199392134966));
#22540=CARTESIAN_POINT('Ctrl Pts',(5.18596130980479,-3.03436470122026,-2.8601112379612));
#22541=CARTESIAN_POINT('Ctrl Pts',(5.14638857315078,-3.58729638923753,-1.67810647154643));
#22542=CARTESIAN_POINT('Ctrl Pts',(5.12897899697745,-3.83055240727213,-1.15809689530562));
#22543=CARTESIAN_POINT('Ctrl Pts',(5.11156942080411,-3.94963463796052,-0.579999886766972));
#22544=CARTESIAN_POINT('Ctrl Pts',(5.09415984463078,-3.94797828517504,-0.00125412662908497));
#22545=CARTESIAN_POINT('Ctrl Pts',(4.98884015536925,-3.94827688052699,-0.00165327621010028));
#22546=CARTESIAN_POINT('Ctrl Pts',(5.005439735774,-3.95036800186029,-0.553368034879958));
#22547=CARTESIAN_POINT('Ctrl Pts',(5.02203931617875,-3.84251013030004,-1.10430146613177));
#22548=CARTESIAN_POINT('Ctrl Pts',(5.0386388965835,-3.62071269423261,-1.60473575307272));
#22549=CARTESIAN_POINT('Ctrl Pts',(5.07821163323751,-3.0919564658209,-2.79775110447809));
#22550=CARTESIAN_POINT('Ctrl Pts',(5.11778436989152,-1.9156514350787,-3.70376640845788));
#22551=CARTESIAN_POINT('Ctrl Pts',(5.15735710654554,-0.627178281783331,
-3.91042000995114));
#22552=CARTESIAN_POINT('Ctrl Pts',(5.19692984319955,0.661294871512074,-4.11707361144442));
#22553=CARTESIAN_POINT('Ctrl Pts',(5.23650257985356,2.06193614736065,-3.62436551045113));
#22554=CARTESIAN_POINT('Ctrl Pts',(5.27607531650758,2.93726099984076,-2.65654570263367));
#22555=CARTESIAN_POINT('Ctrl Pts',(5.31564805316159,3.81258585232085,-1.68872589481625));
#22556=CARTESIAN_POINT('Ctrl Pts',(5.3552207898156,4.16259428143251,-0.24579438017468));
#22557=CARTESIAN_POINT('Ctrl Pts',(5.39479352646961,3.82798428148137,1.01551641645942));
#22558=CARTESIAN_POINT('Ctrl Pts',(5.43436626312363,3.49337428153023,2.27682721309352));
#22559=CARTESIAN_POINT('Ctrl Pts',(5.47393899977764,2.4741458525163,3.35651729172016));
#22560=CARTESIAN_POINT('Ctrl Pts',(5.51351173643165,1.23418820252157,3.76317907255602));
#22561=CARTESIAN_POINT('Ctrl Pts',(5.55308447308566,-0.00576944747316441,
4.16984085339188));
#22562=CARTESIAN_POINT('Ctrl Pts',(5.59265720973968,-1.4664563184487,3.90347433643695));
#22563=CARTESIAN_POINT('Ctrl Pts',(5.63222994639369,-2.48305885483325,3.08531294600745));
#22564=CARTESIAN_POINT('Ctrl Pts',(5.66776668271888,-3.39597869150952,2.35059535855969));
#22565=CARTESIAN_POINT('Ctrl Pts',(5.70330341904407,-3.95077870340937,1.17089768960724));
#22566=CARTESIAN_POINT('Ctrl Pts',(5.73884015536925,-3.95875693366943,-0.00224257783873754));
#22567=CARTESIAN_POINT('Origin',(4.7,0.,0.));
#22568=CARTESIAN_POINT('',(6.59415984463077,-3.95548544114442,0.00341059480280986));
#22569=CARTESIAN_POINT('',(6.48884015536925,-3.95468133138785,0.0035131856141757));
#22570=CARTESIAN_POINT('',(4.7,-3.954,-4.84225344382863E-16));
#22571=CARTESIAN_POINT('Ctrl Pts',(6.59415984463077,-3.95548544114442,0.00341059480280986));
#22572=CARTESIAN_POINT('Ctrl Pts',(6.58644226065226,-3.95780309731958,0.258732729269525));
#22573=CARTESIAN_POINT('Ctrl Pts',(6.57872467667375,-3.93518375266648,0.51364602629909));
#22574=CARTESIAN_POINT('Ctrl Pts',(6.57100709269525,-3.88613019748507,0.763366754762944));
#22575=CARTESIAN_POINT('Ctrl Pts',(6.53143435604123,-3.63460285077364,2.04383647845702));
#22576=CARTESIAN_POINT('Ctrl Pts',(6.49186161938722,-2.68805792945867,3.18778136035047));
#22577=CARTESIAN_POINT('Ctrl Pts',(6.4522888827332,-1.47730364243954,3.6745490420074));
#22578=CARTESIAN_POINT('Ctrl Pts',(6.41271614607919,-0.266549355420404,
4.16131672366433));
#22579=CARTESIAN_POINT('Ctrl Pts',(6.37314340942518,1.20841429730289,3.99090720508476));
#22580=CARTESIAN_POINT('Ctrl Pts',(6.33357067277117,2.27627585959928,3.24088027009456));
#22581=CARTESIAN_POINT('Ctrl Pts',(6.29399793611716,3.3441374218957,2.49085333510434));
#22582=CARTESIAN_POINT('Ctrl Pts',(6.25442519946314,4.00489689376518,1.16120898370345));
#22583=CARTESIAN_POINT('Ctrl Pts',(6.21485246280913,3.95781777746819,-0.142881609871119));
#22584=CARTESIAN_POINT('Ctrl Pts',(6.17527972615511,3.91073866117121,-1.44697220344565));
#22585=CARTESIAN_POINT('Ctrl Pts',(6.1357069895011,3.15582095670779,-2.72550903919386));
#22586=CARTESIAN_POINT('Ctrl Pts',(6.09613425284709,2.03665611631933,-3.39658189625124));
#22587=CARTESIAN_POINT('Ctrl Pts',(6.05656151619308,0.917491275930869,-4.06765475330863));
#22588=CARTESIAN_POINT('Ctrl Pts',(6.01698877953907,-0.565920700382629,
-4.13126363167517));
#22589=CARTESIAN_POINT('Ctrl Pts',(5.97741604288505,-1.73842320654302,-3.55845773742436));
#22590=CARTESIAN_POINT('Ctrl Pts',(5.93784330623104,-2.91092571270342,-2.98565184317355));
#22591=CARTESIAN_POINT('Ctrl Pts',(5.89827056957702,-3.77251874871071,-1.77643117630538));
#22592=CARTESIAN_POINT('Ctrl Pts',(5.85869783292301,-3.93105890511442,-0.481157561099551));
#22593=CARTESIAN_POINT('Ctrl Pts',(5.8538518368256,-3.9504734072231,-0.32254101306424));
#22594=CARTESIAN_POINT('Ctrl Pts',(5.84900584072818,-3.95934496431545,-0.162634019417884));
#22595=CARTESIAN_POINT('Ctrl Pts',(5.84415984463077,-3.95812868148667,-0.00259109635525723));
#22596=CARTESIAN_POINT('Ctrl Pts',(5.73884015536925,-3.95875693366943,-0.00224257783873754));
#22597=CARTESIAN_POINT('Ctrl Pts',(5.74287615569808,-3.95966304220056,-0.135479194219172));
#22598=CARTESIAN_POINT('Ctrl Pts',(5.74691215602691,-3.95351583846345,-0.268631228379135));
#22599=CARTESIAN_POINT('Ctrl Pts',(5.75094815635573,-3.94003888469953,-0.401037203290042));
#22600=CARTESIAN_POINT('Ctrl Pts',(5.79052089300975,-3.80789817638765,-1.69926969825382));
#22601=CARTESIAN_POINT('Ctrl Pts',(5.83009362966376,-2.97109855797036,-2.92577842427728));
#22602=CARTESIAN_POINT('Ctrl Pts',(5.86966636631777,-1.81049902166246,-3.52233311086931));
#22603=CARTESIAN_POINT('Ctrl Pts',(5.90923910297178,-0.649899485354549,
-4.11888779746134));
#22604=CARTESIAN_POINT('Ctrl Pts',(5.9488118396258,0.834499968843993,-4.08548844462194));
#22605=CARTESIAN_POINT('Ctrl Pts',(5.98838457627981,1.96709329651415,-3.43733635453036));
#22606=CARTESIAN_POINT('Ctrl Pts',(6.02795731293382,3.09968662418432,-2.78918426443878));
#22607=CARTESIAN_POINT('Ctrl Pts',(6.06753004958783,3.88047382532609,-1.52627943709504));
#22608=CARTESIAN_POINT('Ctrl Pts',(6.10710278624184,3.95408926638018,-0.223417378160364));
#22609=CARTESIAN_POINT('Ctrl Pts',(6.14667552289586,4.02770470743426,1.07944468077433));
#22610=CARTESIAN_POINT('Ctrl Pts',(6.18624825954988,3.3941483884006,2.42226397129993));
#22611=CARTESIAN_POINT('Ctrl Pts',(6.22582099620389,2.34177562860268,3.19387290865644));
#22612=CARTESIAN_POINT('Ctrl Pts',(6.2653937328579,1.28940286880478,3.96548184601292));
#22613=CARTESIAN_POINT('Ctrl Pts',(6.30496646951191,-0.181786331757368,
4.16588043020035));
#22614=CARTESIAN_POINT('Ctrl Pts',(6.34453920616592,-1.40219841215079,3.70385972524997));
#22615=CARTESIAN_POINT('Ctrl Pts',(6.38411194281993,-2.62261049254421,3.2418390202996));
#22616=CARTESIAN_POINT('Ctrl Pts',(6.42368467947395,-3.59224545276892,2.11739902621141));
#22617=CARTESIAN_POINT('Ctrl Pts',(6.46325741612797,-3.86978593841946,0.842314693079716));
#22618=CARTESIAN_POINT('Ctrl Pts',(6.47178499587506,-3.92959349343203,0.567545135691775));
#22619=CARTESIAN_POINT('Ctrl Pts',(6.48031257562216,-3.95726260853577,0.285780183576929));
#22620=CARTESIAN_POINT('Ctrl Pts',(6.48884015536925,-3.95468133138785,0.0035131856141757));
#22621=CARTESIAN_POINT('Origin',(4.7,0.,0.));
#22622=CARTESIAN_POINT('',(7.34415984463077,-3.94761516686083,-0.000266384231551453));
#22623=CARTESIAN_POINT('',(7.23884015536925,-3.94771372514716,-0.000698679637915435));
#22624=CARTESIAN_POINT('',(4.7,-3.954,-4.84225344382863E-16));
#22625=CARTESIAN_POINT('Ctrl Pts',(7.34415984463077,-3.94761516686083,-0.000266384231551453));
#22626=CARTESIAN_POINT('Ctrl Pts',(7.32387868057634,-3.94720746447042,0.674094403609092));
#22627=CARTESIAN_POINT('Ctrl Pts',(7.30359751652191,-3.78327622808021,1.34864110485744));
#22628=CARTESIAN_POINT('Ctrl Pts',(7.28331635246748,-3.45695268116967,1.93241167307498));
#22629=CARTESIAN_POINT('Ctrl Pts',(7.24374361581347,-2.82022809518258,3.07146852900473));
#22630=CARTESIAN_POINT('Ctrl Pts',(7.20417087915945,-1.56524247678311,3.8649219167271));
#22631=CARTESIAN_POINT('Ctrl Pts',(7.16459814250544,-0.26318700166963,3.95164134458515));
#22632=CARTESIAN_POINT('Ctrl Pts',(7.12502540585142,1.0388684734438,4.0383607724432));
#22633=CARTESIAN_POINT('Ctrl Pts',(7.08545266919741,2.38799380527123,3.41834624043699));
#22634=CARTESIAN_POINT('Ctrl Pts',(7.0458799325434,3.17015129238174,2.37378969108322));
#22635=CARTESIAN_POINT('Ctrl Pts',(7.00630719588939,3.95230877949225,1.32923314172946));
#22636=CARTESIAN_POINT('Ctrl Pts',(6.96673445923537,4.16749842188584,-0.139865424971873));
#22637=CARTESIAN_POINT('Ctrl Pts',(6.92716172258136,3.71777931646781,-1.36486397422117));
#22638=CARTESIAN_POINT('Ctrl Pts',(6.88758898592735,3.26806021104977,-2.58986252347049));
#22639=CARTESIAN_POINT('Ctrl Pts',(6.84801624927334,2.15343235782014,-3.57076105526773));
#22640=CARTESIAN_POINT('Ctrl Pts',(6.80844351261932,0.881204832371534,-3.86111573997565));
#22641=CARTESIAN_POINT('Ctrl Pts',(6.76887077596531,-0.391022693077072,
-4.15147042468356));
#22642=CARTESIAN_POINT('Ctrl Pts',(6.72929803931129,-1.82084989074469,-3.75128126230207));
#22643=CARTESIAN_POINT('Ctrl Pts',(6.68972530265728,-2.75750860352453,-2.84268939836396));
#22644=CARTESIAN_POINT('Ctrl Pts',(6.65787014998178,-3.51149755711427,-2.11129361953467));
#22645=CARTESIAN_POINT('Ctrl Pts',(6.62601499730628,-3.94591906758573,-1.05045880234535));
#22646=CARTESIAN_POINT('Ctrl Pts',(6.59415984463077,-3.95548544114442,0.00341059480280986));
#22647=CARTESIAN_POINT('Ctrl Pts',(6.48884015536925,-3.95468133138785,0.0035131856141757));
#22648=CARTESIAN_POINT('Ctrl Pts',(6.51988531227617,-3.94528403972316,-1.02409646463657));
#22649=CARTESIAN_POINT('Ctrl Pts',(6.55093046918308,-3.5349580443317,-2.05836006467214));
#22650=CARTESIAN_POINT('Ctrl Pts',(6.58197562609,-2.81480309023937,-2.78596855950419));
#22651=CARTESIAN_POINT('Ctrl Pts',(6.62154836274401,-1.89683374533234,-3.71343880678121));
#22652=CARTESIAN_POINT('Ctrl Pts',(6.66112109939803,-0.475449044441877,
-4.14265062915996));
#22653=CARTESIAN_POINT('Ctrl Pts',(6.70069383605204,0.802425353270519,-3.87825357652071));
#22654=CARTESIAN_POINT('Ctrl Pts',(6.74026657270606,2.08029975098288,-3.61385652388146));
#22655=CARTESIAN_POINT('Ctrl Pts',(6.77983930936007,3.21466384551719,-2.65585059622425));
#22656=CARTESIAN_POINT('Ctrl Pts',(6.81941204601408,3.68922585525657,-1.4402603376728));
#22657=CARTESIAN_POINT('Ctrl Pts',(6.85898478266809,4.16378786499596,-0.224670079121361));
#22658=CARTESIAN_POINT('Ctrl Pts',(6.89855751932211,3.97854778994043,1.24850451032431));
#22659=CARTESIAN_POINT('Ctrl Pts',(6.93813025597612,3.21781535819058,2.30876624454704));
#22660=CARTESIAN_POINT('Ctrl Pts',(6.97770299263014,2.45708292644072,3.36902797876977));
#22661=CARTESIAN_POINT('Ctrl Pts',(7.01727572928414,1.12085813799653,4.01637685776957));
#22662=CARTESIAN_POINT('Ctrl Pts',(7.05684846593816,-0.182692828407551,
3.95618004921609));
#22663=CARTESIAN_POINT('Ctrl Pts',(7.09642120259217,-1.48624379481167,3.89598324066261));
#22664=CARTESIAN_POINT('Ctrl Pts',(7.13599393924619,-2.7571209391757,3.12824074455581));
#22665=CARTESIAN_POINT('Ctrl Pts',(7.1755666759002,-3.41690025439169,2.00238105836652));
#22666=CARTESIAN_POINT('Ctrl Pts',(7.19665783572322,-3.76854414262731,1.40232939180324));
#22667=CARTESIAN_POINT('Ctrl Pts',(7.21774899554623,-3.94660011203609,0.700551267122433));
#22668=CARTESIAN_POINT('Ctrl Pts',(7.23884015536925,-3.94771372514716,-0.000698679637915435));
#22669=CARTESIAN_POINT('Origin',(4.7,0.,0.));
#22670=CARTESIAN_POINT('',(8.09415984463078,-3.95644716314161,-0.00320656848566359));
#22671=CARTESIAN_POINT('',(7.98884015536925,-3.95720150084823,-0.00297693462621818));
#22672=CARTESIAN_POINT('',(4.7,-3.954,-4.84225344382863E-16));
#22673=CARTESIAN_POINT('Ctrl Pts',(8.09415984463078,-3.95644716314161,-0.00320656848566359));
#22674=CARTESIAN_POINT('Ctrl Pts',(8.06131510050042,-3.94689655284687,1.08271904018544));
#22675=CARTESIAN_POINT('Ctrl Pts',(8.02847035637007,-3.48188740146714,2.17583507877882));
#22676=CARTESIAN_POINT('Ctrl Pts',(7.99562561223971,-2.68596213185717,2.91038556557579));
#22677=CARTESIAN_POINT('Ctrl Pts',(7.9560528755857,-1.72699770925295,3.79540305445398));
#22678=CARTESIAN_POINT('Ctrl Pts',(7.91648013893168,-0.287660578712081,
4.15991067512015));
#22679=CARTESIAN_POINT('Ctrl Pts',(7.87690740227767,0.976952774382327,3.8380072942491));
#22680=CARTESIAN_POINT('Ctrl Pts',(7.83733466562366,2.24156612747672,3.51610391337806));
#22681=CARTESIAN_POINT('Ctrl Pts',(7.79776192896965,3.33145570312463,2.50778953096983));
#22682=CARTESIAN_POINT('Ctrl Pts',(7.75818919231564,3.75057174667662,1.27198596183832));
#22683=CARTESIAN_POINT('Ctrl Pts',(7.71861645566162,4.16968779022862,0.0361823927067614));
#22684=CARTESIAN_POINT('Ctrl Pts',(7.6790437190076,3.91803030168461,-1.42711036314813));
#22685=CARTESIAN_POINT('Ctrl Pts',(7.63947098235359,3.11013807308118,-2.45189271389543));
#22686=CARTESIAN_POINT('Ctrl Pts',(7.59989824569957,2.30224584447777,-3.4766750646427));
#22687=CARTESIAN_POINT('Ctrl Pts',(7.56032550904557,0.938118875814986,-4.06294701028245));
#22688=CARTESIAN_POINT('Ctrl Pts',(7.52075277239156,-0.361377322092827,
-3.9438741289701));
#22689=CARTESIAN_POINT('Ctrl Pts',(7.48118003573754,-1.66087352000064,-3.82480124765774));
#22690=CARTESIAN_POINT('Ctrl Pts',(7.44160729908353,-2.89573894715346,-3.00038353939327));
#22691=CARTESIAN_POINT('Ctrl Pts',(7.40203456242951,-3.50393988394249,-1.8458445231925));
#22692=CARTESIAN_POINT('Ctrl Pts',(7.38274298982993,-3.80043574243673,-1.28301073575904));
#22693=CARTESIAN_POINT('Ctrl Pts',(7.36345141723035,-3.94800297597488,-0.641722666623542));
#22694=CARTESIAN_POINT('Ctrl Pts',(7.34415984463077,-3.94761516686083,-0.000266384231551453));
#22695=CARTESIAN_POINT('Ctrl Pts',(7.23884015536925,-3.94771372514716,-0.000698679637915435));
#22696=CARTESIAN_POINT('Ctrl Pts',(7.25732173220024,-3.94868955229203,-0.615183842025179));
#22697=CARTESIAN_POINT('Ctrl Pts',(7.27580330903124,-3.81379996271696,-1.22926344231433));
#22698=CARTESIAN_POINT('Ctrl Pts',(7.29428488586223,-3.5407879365703,-1.77413585714432));
#22699=CARTESIAN_POINT('Ctrl Pts',(7.33385762251625,-2.95621481746495,-2.94081621019416));
#22700=CARTESIAN_POINT('Ctrl Pts',(7.37343035917026,-1.73838709318626,-3.79020004002209));
#22701=CARTESIAN_POINT('Ctrl Pts',(7.41300309582428,-0.441583983695238,
-3.93570080630005));
#22702=CARTESIAN_POINT('Ctrl Pts',(7.45257583247829,0.855219125795781,-4.081201572578));
#22703=CARTESIAN_POINT('Ctrl Pts',(7.4921485691323,2.23099762049913,-3.52281927530597));
#22704=CARTESIAN_POINT('Ctrl Pts',(7.53172130578631,3.05958294169278,-2.51469470796547));
#22705=CARTESIAN_POINT('Ctrl Pts',(7.57129404244033,3.88816826288645,-1.50657014062495));
#22706=CARTESIAN_POINT('Ctrl Pts',(7.61086677909435,4.1695604105704,-0.0487033032159304));
#22707=CARTESIAN_POINT('Ctrl Pts',(7.65043951574836,3.77568723052116,1.19537575207398));
#22708=CARTESIAN_POINT('Ctrl Pts',(7.69001225240237,3.38181405047194,2.43945480736386));
#22709=CARTESIAN_POINT('Ctrl Pts',(7.72958498905637,2.31267554268956,3.46974608053465));
#22710=CARTESIAN_POINT('Ctrl Pts',(7.76915772571039,1.05487687004705,3.81732524687205));
#22711=CARTESIAN_POINT('Ctrl Pts',(7.8087304623644,-0.202921802595454,4.16490441320944));
#22712=CARTESIAN_POINT('Ctrl Pts',(7.84830319901842,-1.64938064009809,3.82977147271344));
#22713=CARTESIAN_POINT('Ctrl Pts',(7.88787593567243,-2.62616180027425,2.96445803649627));
#22714=CARTESIAN_POINT('Ctrl Pts',(7.92153067557138,-3.45686795464837,2.22854990657432));
#22715=CARTESIAN_POINT('Ctrl Pts',(7.95518541547031,-3.94787044850959,1.10917825725707));
#22716=CARTESIAN_POINT('Ctrl Pts',(7.98884015536925,-3.95720150084823,-0.00297693462621818));
#22717=CARTESIAN_POINT('Origin',(4.7,0.,0.));
#22718=CARTESIAN_POINT('',(8.84415984463078,-3.95727591145965,0.00295051159254288));
#22719=CARTESIAN_POINT('',(8.73884015536925,-3.95652560052937,0.00318574057616234));
#22720=CARTESIAN_POINT('',(4.7,-3.954,-4.84225344382863E-16));
#22721=CARTESIAN_POINT('Ctrl Pts',(8.84415984463078,-3.95727591145965,0.00295051159254288));
#22722=CARTESIAN_POINT('Ctrl Pts',(8.83832425707851,-3.95888409829544,0.195783997048772));
#22723=CARTESIAN_POINT('Ctrl Pts',(8.83248866952625,-3.94599938707022,0.3884017661895));
#22724=CARTESIAN_POINT('Ctrl Pts',(8.82665308197398,-3.91787743633585,0.578768613465758));
#22725=CARTESIAN_POINT('Ctrl Pts',(8.78708034531997,-3.72717469378571,1.86969896922656));
#22726=CARTESIAN_POINT('Ctrl Pts',(8.74750760866596,-2.83577652030062,3.05711906219486));
#22727=CARTESIAN_POINT('Ctrl Pts',(8.70793487201194,-1.64939176486137,3.60058932955289));
#22728=CARTESIAN_POINT('Ctrl Pts',(8.66836213535793,-0.463007009422064,
4.14405959691094));
#22729=CARTESIAN_POINT('Ctrl Pts',(8.62878939870392,1.0183643279714,4.04358003865869));
#22730=CARTESIAN_POINT('Ctrl Pts',(8.58921666204991,2.12049441279558,3.3448826824547));
#22731=CARTESIAN_POINT('Ctrl Pts',(8.54964392539589,3.22262449761972,2.64618532625074));
#22732=CARTESIAN_POINT('Ctrl Pts',(8.51007118874188,3.94551332987458,1.34927017209508));
#22733=CARTESIAN_POINT('Ctrl Pts',(8.47049845208787,3.96014700219647,0.0444121050719863));
#22734=CARTESIAN_POINT('Ctrl Pts',(8.43092571543385,3.97478067451836,-1.26044596195111));
#22735=CARTESIAN_POINT('Ctrl Pts',(8.39135297877984,3.28115918690728,-2.57324694184166));
#22736=CARTESIAN_POINT('Ctrl Pts',(8.35178024212583,2.19497577695067,-3.29648571249481));
#22737=CARTESIAN_POINT('Ctrl Pts',(8.31220750547182,1.10879236699404,-4.01972448314798));
#22738=CARTESIAN_POINT('Ctrl Pts',(8.2726347688178,-0.3699529653081,-4.15340104456376));
#22739=CARTESIAN_POINT('Ctrl Pts',(8.23306203216379,-1.56822757915689,-3.63667416385554));
#22740=CARTESIAN_POINT('Ctrl Pts',(8.19348929550978,-2.76650219300569,-3.11994728314731));
#22741=CARTESIAN_POINT('Ctrl Pts',(8.15391655885576,-3.68430608840111,-1.95281696031504));
#22742=CARTESIAN_POINT('Ctrl Pts',(8.11434382220175,-3.90391217876503,-0.666488120353801));
#22743=CARTESIAN_POINT('Ctrl Pts',(8.10761582967809,-3.94124869524191,-0.447791827148448));
#22744=CARTESIAN_POINT('Ctrl Pts',(8.10088783715443,-3.95840353200246,-0.225650054341145));
#22745=CARTESIAN_POINT('Ctrl Pts',(8.09415984463078,-3.95644716314161,-0.00320656848566359));
#22746=CARTESIAN_POINT('Ctrl Pts',(7.98884015536925,-3.95720150084823,-0.00297693462621818));
#22747=CARTESIAN_POINT('Ctrl Pts',(7.99475815212432,-3.95884231392916,-0.198543170956203));
#22748=CARTESIAN_POINT('Ctrl Pts',(8.00067614887939,-3.94558924647289,-0.393886265439571));
#22749=CARTESIAN_POINT('Ctrl Pts',(8.00659414563446,-3.91667037322966,-0.586881963287379));
#22750=CARTESIAN_POINT('Ctrl Pts',(8.04616688228848,-3.72329430315924,-1.87741459491562));
#22751=CARTESIAN_POINT('Ctrl Pts',(8.0857396189425,-2.82943868016865,-3.0629859262337));
#22752=CARTESIAN_POINT('Ctrl Pts',(8.12531235559651,-1.64193083097396,-3.60399783541336));
#22753=CARTESIAN_POINT('Ctrl Pts',(8.16488509225053,-0.454422981779327,
-4.14500974459299));
#22754=CARTESIAN_POINT('Ctrl Pts',(8.20445782890453,1.02673709361936,-4.04146223163425));
#22755=CARTESIAN_POINT('Ctrl Pts',(8.24403056555854,2.12741771398153,-3.34048366581915));
#22756=CARTESIAN_POINT('Ctrl Pts',(8.28360330221256,3.22809833434371,-2.63950510000405));
#22757=CARTESIAN_POINT('Ctrl Pts',(8.32317603886657,3.94829949966936,-1.3410954813326));
#22758=CARTESIAN_POINT('Ctrl Pts',(8.36274877552059,3.9602305609419,-0.0362098819216899));
#22759=CARTESIAN_POINT('Ctrl Pts',(8.4023215121746,3.97216162221444,1.2686757174892));
#22760=CARTESIAN_POINT('Ctrl Pts',(8.44189424882861,3.27582257943385,2.58003729763958));
#22761=CARTESIAN_POINT('Ctrl Pts',(8.48146698548262,2.18814353179743,3.30102486140593));
#22762=CARTESIAN_POINT('Ctrl Pts',(8.52103972213664,1.10046448416096,4.02201242517232));
#22763=CARTESIAN_POINT('Ctrl Pts',(8.56061245879065,-0.37855456833137,4.15262597255467));
#22764=CARTESIAN_POINT('Ctrl Pts',(8.60018519544467,-1.57575640452294,3.63341836360361));
#22765=CARTESIAN_POINT('Ctrl Pts',(8.63975793209868,-2.77295824071448,3.11421075465256));
#22766=CARTESIAN_POINT('Ctrl Pts',(8.67933066875269,-3.68834286060526,1.94518198936815));
#22767=CARTESIAN_POINT('Ctrl Pts',(8.7189034054067,-3.90528428092833,0.658401045337166));
#22768=CARTESIAN_POINT('Ctrl Pts',(8.72554898872755,-3.9417159863498,0.442307575380675));
#22769=CARTESIAN_POINT('Ctrl Pts',(8.7321945720484,-3.95845046258346,0.22289330331233));
#22770=CARTESIAN_POINT('Ctrl Pts',(8.73884015536925,-3.95652560052937,0.00318574057616234));
#22771=CARTESIAN_POINT('Origin',(4.7,0.,0.));
#22772=CARTESIAN_POINT('',(9.59415984463078,-3.94772861144879,0.000742196070642187));
#22773=CARTESIAN_POINT('',(9.48884015536925,-3.9476212151691,0.00031064949736361));
#22774=CARTESIAN_POINT('',(4.7,-3.954,-4.84225344382863E-16));
#22775=CARTESIAN_POINT('Ctrl Pts',(9.59415984463078,-3.94772861144879,0.000742196070642187));
#22776=CARTESIAN_POINT('Ctrl Pts',(9.57576067700259,-3.9487608168787,0.612481575277166));
#22777=CARTESIAN_POINT('Ctrl Pts',(9.5573615093744,-3.81512540423781,1.22379386335884));
#22778=CARTESIAN_POINT('Ctrl Pts',(9.53896234174621,-3.54445481419423,1.7667984560266));
#22779=CARTESIAN_POINT('Ctrl Pts',(9.4993896050922,-2.96229934954316,2.93468703565128));
#22780=CARTESIAN_POINT('Ctrl Pts',(9.45981686843819,-1.74623347451844,3.78659135450272));
#22781=CARTESIAN_POINT('Ctrl Pts',(9.42024413178417,-0.449734525193319,
3.93477770286096));
#22782=CARTESIAN_POINT('Ctrl Pts',(9.38067139513016,0.846764424131798,4.08296405121919));
#22783=CARTESIAN_POINT('Ctrl Pts',(9.34109865847615,2.22369644775731,3.52743242908423));
#22784=CARTESIAN_POINT('Ctrl Pts',(9.30152592182214,3.05436797254543,2.52102618042165));
#22785=CARTESIAN_POINT('Ctrl Pts',(9.26195318516812,3.88503949733354,1.51461993175908));
#22786=CARTESIAN_POINT('Ctrl Pts',(9.22238044851411,4.16945052328425,0.0573390565689048));
#22787=CARTESIAN_POINT('Ctrl Pts',(9.1828077118601,3.77815489108496,-1.18755308641483));
#22788=CARTESIAN_POINT('Ctrl Pts',(9.14323497520609,3.38685925888568,-2.43244522939857));
#22789=CARTESIAN_POINT('Ctrl Pts',(9.10366223855208,2.3198569685364,-3.46494864017587));
#22790=CARTESIAN_POINT('Ctrl Pts',(9.06408950189806,1.06278090997786,-3.81513216697263));
#22791=CARTESIAN_POINT('Ctrl Pts',(9.02451676524405,-0.194295148580706,
-4.1653156937694));
#22792=CARTESIAN_POINT('Ctrl Pts',(8.98494402859004,-1.64144497534855,-3.83317933658557));
#22793=CARTESIAN_POINT('Ctrl Pts',(8.94537129193602,-2.62001623292487,-2.96989084871697));
#22794=CARTESIAN_POINT('Ctrl Pts',(8.91163414283427,-3.45428262981783,-2.23390706554609));
#22795=CARTESIAN_POINT('Ctrl Pts',(8.87789699373252,-3.94797853761737,-1.11187331589373));
#22796=CARTESIAN_POINT('Ctrl Pts',(8.84415984463078,-3.95727591145965,0.00295051159254288));
#22797=CARTESIAN_POINT('Ctrl Pts',(8.73884015536925,-3.95652560052937,0.00318574057616234));
#22798=CARTESIAN_POINT('Ctrl Pts',(8.77176730870242,-3.9469884049304,-1.0854086321664));
#22799=CARTESIAN_POINT('Ctrl Pts',(8.80469446203558,-3.47937430514818,-2.18120313596773));
#22800=CARTESIAN_POINT('Ctrl Pts',(8.83762161536874,-2.67992852017388,-2.91594245109975));
#22801=CARTESIAN_POINT('Ctrl Pts',(8.87719435202275,-1.71913311834099,-3.79897188072816));
#22802=CARTESIAN_POINT('Ctrl Pts',(8.91676708867676,-0.279044093919909,
-4.16049761720741));
#22803=CARTESIAN_POINT('Ctrl Pts',(8.95633982533078,0.984899852510242,-3.83597569490375));
#22804=CARTESIAN_POINT('Ctrl Pts',(8.99591256198479,2.24884379894041,-3.51145377260009));
#22805=CARTESIAN_POINT('Ctrl Pts',(9.03548529863881,3.33664266737961,-2.50088419151347));
#22806=CARTESIAN_POINT('Ctrl Pts',(9.07505803529282,3.75319826269509,-1.26421519223174));
#22807=CARTESIAN_POINT('Ctrl Pts',(9.11463077194684,4.16975385801057,-0.0275461929500335));
#22808=CARTESIAN_POINT('Ctrl Pts',(9.15420350860084,3.91506618020236,1.43522222452681));
#22809=CARTESIAN_POINT('Ctrl Pts',(9.19377624525486,3.10505317445673,2.45832911449284));
#22810=CARTESIAN_POINT('Ctrl Pts',(9.23334898190887,2.29504016871111,3.48143600445886));
#22811=CARTESIAN_POINT('Ctrl Pts',(9.27292171856288,0.92970183502812,4.06488136691408));
#22812=CARTESIAN_POINT('Ctrl Pts',(9.3124944552169,-0.369544977977794,3.94311726437579));
#22813=CARTESIAN_POINT('Ctrl Pts',(9.35206719187091,-1.66879179098376,3.82135316183748));
#22814=CARTESIAN_POINT('Ctrl Pts',(9.39163992852492,-2.90194708331263,2.99437959430555));
#22815=CARTESIAN_POINT('Ctrl Pts',(9.43121266517893,-3.50775548206036,1.83858334851659));
#22816=CARTESIAN_POINT('Ctrl Pts',(9.45042182857571,-3.80182340615735,1.27754358184973));
#22817=CARTESIAN_POINT('Ctrl Pts',(9.46963099197248,-3.94807157344821,0.639024371465793));
#22818=CARTESIAN_POINT('Ctrl Pts',(9.48884015536925,-3.9476212151691,0.00031064949736361));
#22819=CARTESIAN_POINT('Origin',(4.7,0.,0.));
#22820=CARTESIAN_POINT('',(10.3441598446308,-3.95459914581543,-0.00352034347287922));
#22821=CARTESIAN_POINT('',(10.2388401553693,-3.95540412882742,-0.0034237005329492));
#22822=CARTESIAN_POINT('',(4.7,-3.954,-4.84225344382863E-16));
#22823=CARTESIAN_POINT('Ctrl Pts',(10.3441598446308,-3.95459914581543,-0.00352034347287922));
#22824=CARTESIAN_POINT('Ctrl Pts',(10.3131970969267,-3.94522735882427,1.02141614396006));
#22825=CARTESIAN_POINT('Ctrl Pts',(10.2822343492226,-3.53730596752864,2.05296951176746));
#22826=CARTESIAN_POINT('Ctrl Pts',(10.2512716015185,-2.82056721260417,2.78013260713677));
#22827=CARTESIAN_POINT('Ctrl Pts',(10.2116988648644,-1.90452079871997,3.70950211763882));
#22828=CARTESIAN_POINT('Ctrl Pts',(10.1721261282104,-0.484028140502754,
4.14165693807744));
#22829=CARTESIAN_POINT('Ctrl Pts',(10.1325533915564,0.794391105071104,3.87990714918108));
#22830=CARTESIAN_POINT('Ctrl Pts',(10.0929806549024,2.07281035064496,3.61815736028473));
#22831=CARTESIAN_POINT('Ctrl Pts',(10.0534079182484,3.20915618357542,2.66250296205341));
#22832=CARTESIAN_POINT('Ctrl Pts',(10.0138351815944,3.68623485853561,1.44789822908918));
#22833=CARTESIAN_POINT('Ctrl Pts',(9.97426244494036,4.1633135334958,0.233293496124942));
#22834=CARTESIAN_POINT('Ctrl Pts',(9.93468970828635,3.98112505048568,-1.24026157157228));
#22835=CARTESIAN_POINT('Ctrl Pts',(9.89511697163234,3.22259024324513,-2.30209661791679));
#22836=CARTESIAN_POINT('Ctrl Pts',(9.85554423497832,2.46405543600457,-3.36393166426134));
#22837=CARTESIAN_POINT('Ctrl Pts',(9.8159714983243,1.12917430453357,-4.01404668925322));
#22838=CARTESIAN_POINT('Ctrl Pts',(9.77639876167029,-0.174498521279079,
-3.95654988344063));
#22839=CARTESIAN_POINT('Ctrl Pts',(9.73682602501627,-1.47817134709166,-3.89905307762803));
#22840=CARTESIAN_POINT('Ctrl Pts',(9.69725328836227,-2.75063586724586,-3.13394444101105));
#22841=CARTESIAN_POINT('Ctrl Pts',(9.65768055170826,-3.41274560018428,-2.00945370250361));
#22842=CARTESIAN_POINT('Ctrl Pts',(9.63650698268243,-3.76701036219998,-1.40778992375466));
#22843=CARTESIAN_POINT('Ctrl Pts',(9.61533341365661,-3.94654076027199,-0.703241061932939));
#22844=CARTESIAN_POINT('Ctrl Pts',(9.59415984463078,-3.94772861144879,0.000742196070642187));
#22845=CARTESIAN_POINT('Ctrl Pts',(9.48884015536925,-3.9476212151691,0.00031064949736361));
#22846=CARTESIAN_POINT('Ctrl Pts',(9.5092037286265,-3.94714379178427,-0.676787743548417));
#22847=CARTESIAN_POINT('Ctrl Pts',(9.52956730188374,-3.78180578893861,-1.35410472974234));
#22848=CARTESIAN_POINT('Ctrl Pts',(9.54993087514098,-3.45294297697788,-1.93956749021687));
#22849=CARTESIAN_POINT('Ctrl Pts',(9.58950361179499,-2.81386056798107,-3.07730315911534));
#22850=CARTESIAN_POINT('Ctrl Pts',(9.629076348449,-1.55723424482083,-3.86815557286639));
#22851=CARTESIAN_POINT('Ctrl Pts',(9.66864908510301,-0.255001929666197,
-3.95217804093306));
#22852=CARTESIAN_POINT('Ctrl Pts',(9.70822182175703,1.04723038548845,-4.03620050899974));
#22853=CARTESIAN_POINT('Ctrl Pts',(9.74779455841104,2.39506869263753,-3.41339303138206));
#22854=CARTESIAN_POINT('Ctrl Pts',(9.78736729506505,3.17506106370751,-2.36721872523338));
#22855=CARTESIAN_POINT('Ctrl Pts',(9.82694003171907,3.95505343477749,-1.32104441908469));
#22856=CARTESIAN_POINT('Ctrl Pts',(9.86651276837308,4.16719986976838,0.148496715594994));
#22857=CARTESIAN_POINT('Ctrl Pts',(9.90608550502709,3.7149445437798,1.37256121466685));
#22858=CARTESIAN_POINT('Ctrl Pts',(9.94565824168111,3.2626892177912,2.59662571373873));
#22859=CARTESIAN_POINT('Ctrl Pts',(9.98523097833512,2.14603213082312,3.57521357720275));
#22860=CARTESIAN_POINT('Ctrl Pts',(10.0248037149891,0.873205939095632,3.86293264752249));
#22861=CARTESIAN_POINT('Ctrl Pts',(10.0643764516431,-0.399620252631823,
4.15065171784221));
#22862=CARTESIAN_POINT('Ctrl Pts',(10.1039491882972,-1.82861554911865,3.74750199501769));
#22863=CARTESIAN_POINT('Ctrl Pts',(10.1435219249512,-2.76339042278715,2.83697208703492));
#22864=CARTESIAN_POINT('Ctrl Pts',(10.1752946684239,-3.51391628420185,2.10591238187753));
#22865=CARTESIAN_POINT('Ctrl Pts',(10.2070674118966,-3.94584788289007,1.04777510454963));
#22866=CARTESIAN_POINT('Ctrl Pts',(10.2388401553693,-3.95540412882742,-0.0034237005329492));
#22867=CARTESIAN_POINT('Origin',(4.7,0.,0.));
#22868=CARTESIAN_POINT('',(11.0941598446308,-3.95881660301891,0.00220458637196837));
#22869=CARTESIAN_POINT('',(10.9888401553692,-3.95819583346249,0.00255778193754717));
#22870=CARTESIAN_POINT('',(4.7,-3.954,-4.84225344382863E-16));
#22871=CARTESIAN_POINT('Ctrl Pts',(11.0941598446308,-3.95881660301891,0.00220458637196837));
#22872=CARTESIAN_POINT('Ctrl Pts',(11.0902062535048,-3.95969225385185,0.132715516968071));
#22873=CARTESIAN_POINT('Ctrl Pts',(11.0862526623788,-3.95379409173705,0.263146353242184));
#22874=CARTESIAN_POINT('Ctrl Pts',(11.0822990712527,-3.94086098162676,0.392875855157525));
#22875=CARTESIAN_POINT('Ctrl Pts',(11.0427263345987,-3.81140941615156,1.69137922890495));
#22876=CARTESIAN_POINT('Ctrl Pts',(11.0031535979447,-2.97715191209434,2.9196184555242));
#22877=CARTESIAN_POINT('Ctrl Pts',(10.9635808612907,-1.81779044977045,3.51857564858477));
#22878=CARTESIAN_POINT('Ctrl Pts',(10.9240081246367,-0.658428987446535,
4.11753284164536));
#22879=CARTESIAN_POINT('Ctrl Pts',(10.8844353879827,0.826036433144062,4.08720800114722));
#22880=CARTESIAN_POINT('Ctrl Pts',(10.8448626513286,1.95996974379351,3.44140310302274));
#22881=CARTESIAN_POINT('Ctrl Pts',(10.8052899146746,3.09390305444297,2.79559820489827));
#22882=CARTESIAN_POINT('Ctrl Pts',(10.7657171780206,3.87730425515128,1.53431324914745));
#22883=CARTESIAN_POINT('Ctrl Pts',(10.7261444413666,3.95361798280149,0.231606476917969));
#22884=CARTESIAN_POINT('Ctrl Pts',(10.6865717047126,4.0299317104517,-1.07110029531144));
#22885=CARTESIAN_POINT('Ctrl Pts',(10.6469989680586,3.39915796504391,-2.41522888401951));
#22886=CARTESIAN_POINT('Ctrl Pts',(10.6074262314046,2.34838561194535,-3.1890157935783));
#22887=CARTESIAN_POINT('Ctrl Pts',(10.5678534947506,1.29761325884674,-3.96280270313713));
#22888=CARTESIAN_POINT('Ctrl Pts',(10.5282807580965,-0.17315770194269,-4.16624793354662));
#22889=CARTESIAN_POINT('Ctrl Pts',(10.4887080214425,-1.39452406614718,-3.70675590550802));
#22890=CARTESIAN_POINT('Ctrl Pts',(10.4491352847885,-2.61589043035163,-3.24726387746944));
#22891=CARTESIAN_POINT('Ctrl Pts',(10.4095625481345,-3.58785219797115,-2.12483459098281));
#22892=CARTESIAN_POINT('Ctrl Pts',(10.3699898114805,-3.86803299700534,-0.850327847456766));
#22893=CARTESIAN_POINT('Ctrl Pts',(10.3613798225306,-3.92899298581659,-0.573028628191791));
#22894=CARTESIAN_POINT('Ctrl Pts',(10.3527698335807,-3.95720521240893,-0.288530314664122));
#22895=CARTESIAN_POINT('Ctrl Pts',(10.3441598446308,-3.95459914581543,-0.00352034347287922));
#22896=CARTESIAN_POINT('Ctrl Pts',(10.2388401553693,-3.95540412882742,-0.0034237005329492));
#22897=CARTESIAN_POINT('Ctrl Pts',(10.2466401485506,-3.95775012243715,-0.261485882632503));
#22898=CARTESIAN_POINT('Ctrl Pts',(10.2544401417319,-3.9346408534935,-0.519129904364567));
#22899=CARTESIAN_POINT('Ctrl Pts',(10.2622401349132,-3.88454086821667,-0.77141395795088));
#22900=CARTESIAN_POINT('Ctrl Pts',(10.3018128715672,-3.63036198912756,-2.0513600018129));
#22901=CARTESIAN_POINT('Ctrl Pts',(10.3413856082212,-2.68144978009919,-3.19334199639593));
#22902=CARTESIAN_POINT('Ctrl Pts',(10.3809583448752,-1.46968989174215,-3.67760096713576));
#22903=CARTESIAN_POINT('Ctrl Pts',(10.4205310815293,-0.257930003385074,
-4.1618599378756));
#22904=CARTESIAN_POINT('Ctrl Pts',(10.4601038181833,1.21667756430069,-3.9883958847722));
#22905=CARTESIAN_POINT('Ctrl Pts',(10.4996765548373,2.28298342288284,-3.23615882524473));
#22906=CARTESIAN_POINT('Ctrl Pts',(10.5392492914913,3.34928928146496,-2.48392176571727));
#22907=CARTESIAN_POINT('Ctrl Pts',(10.5788220281453,4.00729343094349,-1.15291169976578));
#22908=CARTESIAN_POINT('Ctrl Pts',(10.6183947647993,3.95751342447232,0.151078610293575));
#22909=CARTESIAN_POINT('Ctrl Pts',(10.6579675014533,3.90773341800116,1.45506892035293));
#22910=CARTESIAN_POINT('Ctrl Pts',(10.6975402381073,3.15016925558029,2.73203947452015));
#22911=CARTESIAN_POINT('Ctrl Pts',(10.7371129747614,2.02961689204451,3.40079292561223));
#22912=CARTESIAN_POINT('Ctrl Pts',(10.7766857114154,0.909064528508733,4.06954637670431));
#22913=CARTESIAN_POINT('Ctrl Pts',(10.8162584480694,-0.574476036141954,
4.13008272472125));
#22914=CARTESIAN_POINT('Ctrl Pts',(10.8558311847234,-1.74578967043865,3.55484959990684));
#22915=CARTESIAN_POINT('Ctrl Pts',(10.8954039213774,-2.91710330473538,2.97961647509242));
#22916=CARTESIAN_POINT('Ctrl Pts',(10.9349766580314,-3.77619000867811,1.76861387744662));
#22917=CARTESIAN_POINT('Ctrl Pts',(10.9745493946854,-3.93204709884383,0.473014654994837));
#22918=CARTESIAN_POINT('Ctrl Pts',(10.97931298158,-3.9508084698007,0.317056285709203));
#22919=CARTESIAN_POINT('Ctrl Pts',(10.9840765684746,-3.95937986467358,0.159872089799277));
#22920=CARTESIAN_POINT('Ctrl Pts',(10.9888401553692,-3.95819583346249,0.00255778193754717));
#22921=CARTESIAN_POINT('Origin',(4.7,0.,0.));
#22922=CARTESIAN_POINT('',(11.8441598446308,-3.9483118015039,0.00169262224176542));
#22923=CARTESIAN_POINT('',(11.7388401553692,-3.94800490926472,0.00129567598274352));
#22924=CARTESIAN_POINT('',(4.7,-3.954,-4.84225344382863E-16));
#22925=CARTESIAN_POINT('Ctrl Pts',(11.8441598446308,-3.9483118015039,0.00169262224176542));
#22926=CARTESIAN_POINT('Ctrl Pts',(11.8276426734288,-3.95044317207578,0.550656188455528));
#22927=CARTESIAN_POINT('Ctrl Pts',(11.8111255022269,-3.84369304308854,1.09882729481394));
#22928=CARTESIAN_POINT('Ctrl Pts',(11.794608331025,-3.62402854299927,1.59723318054838));
#22929=CARTESIAN_POINT('Ctrl Pts',(11.7550355943709,-3.09774439252394,2.79134109538696));
#22930=CARTESIAN_POINT('Ctrl Pts',(11.7154628577169,-1.92331841462687,3.6997907656419));
#22931=CARTESIAN_POINT('Ctrl Pts',(11.6758901210629,-0.635276061282561,
3.90911256430254));
#22932=CARTESIAN_POINT('Ctrl Pts',(11.6363173844089,0.652766292061783,4.11843436296318));
#22933=CARTESIAN_POINT('Ctrl Pts',(11.5967446477549,2.05442502085337,3.62862829002949));
#22934=CARTESIAN_POINT('Ctrl Pts',(11.5571719111009,2.93175249797369,2.66262351913797));
#22935=CARTESIAN_POINT('Ctrl Pts',(11.5175991744469,3.80907997509398,1.69661874824647));
#22936=CARTESIAN_POINT('Ctrl Pts',(11.4780264377928,4.16207620054304,0.254415279397177));
#22937=CARTESIAN_POINT('Ctrl Pts',(11.4384537011388,3.83007931013461,-1.00758582368442));
#22938=CARTESIAN_POINT('Ctrl Pts',(11.3988809644848,3.49808241972618,-2.26958692676602));
#22939=CARTESIAN_POINT('Ctrl Pts',(11.3593082278308,2.48109241346025,-3.35138566407993));
#22940=CARTESIAN_POINT('Ctrl Pts',(11.3197354911768,1.24197970898019,-3.76061472589476));
#22941=CARTESIAN_POINT('Ctrl Pts',(11.2801627545228,0.00286700450012237,
-4.16984378770958));
#22942=CARTESIAN_POINT('Ctrl Pts',(11.2405900178688,-1.45836839819409,-3.90650317402533));
#22943=CARTESIAN_POINT('Ctrl Pts',(11.2010172812148,-2.47666328609461,-3.09044910674541));
#22944=CARTESIAN_POINT('Ctrl Pts',(11.1653981356868,-3.39322344516725,-2.35592450625361));
#22945=CARTESIAN_POINT('Ctrl Pts',(11.1297789901588,-3.950927589346,-1.17360942213905));
#22946=CARTESIAN_POINT('Ctrl Pts',(11.0941598446308,-3.95881660301891,0.00220458637196837));
#22947=CARTESIAN_POINT('Ctrl Pts',(10.9888401553692,-3.95819583346249,0.00255778193754717));
#22948=CARTESIAN_POINT('Ctrl Pts',(11.0236493051287,-3.9495437146582,-1.14699137562275));
#22949=CARTESIAN_POINT('Ctrl Pts',(11.0584584548881,-3.41997896279796,-2.30348814970156));
#22950=CARTESIAN_POINT('Ctrl Pts',(11.0932676046475,-2.5390593592383,-3.0393938247008));
#22951=CARTESIAN_POINT('Ctrl Pts',(11.1328403413015,-1.53758705307831,-3.87600723468695));
#22952=CARTESIAN_POINT('Ctrl Pts',(11.1724130779555,-0.0820149643695929,
-4.16903820740154));
#22953=CARTESIAN_POINT('Ctrl Pts',(11.2119858146095,1.16517128117612,-3.78511732141781));
#22954=CARTESIAN_POINT('Ctrl Pts',(11.2515585512635,2.4123575267218,-3.4011964354341));
#22955=CARTESIAN_POINT('Ctrl Pts',(11.2911312879175,3.45115792910449,-2.34032369075211));
#22956=CARTESIAN_POINT('Ctrl Pts',(11.3307040245716,3.80877533873865,-1.08534219045179));
#22957=CARTESIAN_POINT('Ctrl Pts',(11.3702767612256,4.16639274837284,0.169639309848643));
#22958=CARTESIAN_POINT('Ctrl Pts',(11.4098494978796,3.84282716525836,1.61872956576745));
#22959=CARTESIAN_POINT('Ctrl Pts',(11.4494222345336,2.98534546091942,2.60239307759696));
#22960=CARTESIAN_POINT('Ctrl Pts',(11.4889949711876,2.12786375658053,3.58605658942642));
#22961=CARTESIAN_POINT('Ctrl Pts',(11.5285677078416,0.736465931017243,4.10429335716664));
#22962=CARTESIAN_POINT('Ctrl Pts',(11.5681404444956,-0.555570511864919,
3.9212343283417));
#22963=CARTESIAN_POINT('Ctrl Pts',(11.6077131811497,-1.84760695474708,3.73817529951676));
#22964=CARTESIAN_POINT('Ctrl Pts',(11.6472859178037,-3.04028201494811,2.85382047412666));
#22965=CARTESIAN_POINT('Ctrl Pts',(11.6868586544577,-3.59076439635125,1.6706730084585));
#22966=CARTESIAN_POINT('Ctrl Pts',(11.7041858214282,-3.83179650439823,1.1526245887188));
#22967=CARTESIAN_POINT('Ctrl Pts',(11.7215129883987,-3.94970869911457,0.577292233503969));
#22968=CARTESIAN_POINT('Ctrl Pts',(11.7388401553692,-3.94800490926472,0.00129567598274352));
#22969=CARTESIAN_POINT('Origin',(4.7,0.,0.));
#22970=CARTESIAN_POINT('',(12.5941598446308,-3.95274743352102,-0.003520024949899));
#22971=CARTESIAN_POINT('',(12.4888401553692,-3.95353526093205,-0.00355836282268518));
#22972=CARTESIAN_POINT('',(4.7,-3.954,-4.84225344382863E-16));
#22973=CARTESIAN_POINT('Ctrl Pts',(12.5941598446308,-3.95274743352102,-0.003520024949899));
#22974=CARTESIAN_POINT('Ctrl Pts',(12.5650790933529,-3.94431242632764,0.960271211073185));
#22975=CARTESIAN_POINT('Ctrl Pts',(12.5359983420751,-3.58899174946445,1.92963147645128));
#22976=CARTESIAN_POINT('Ctrl Pts',(12.5069175907972,-2.94886311311229,2.64366091296727));
#22977=CARTESIAN_POINT('Ctrl Pts',(12.4673448541432,-2.07778376206595,3.61530358424772));
#22978=CARTESIAN_POINT('Ctrl Pts',(12.4277721174892,-0.679313005392218,
4.11413894713976));
#22979=CARTESIAN_POINT('Ctrl Pts',(12.3881993808351,0.610052503064052,3.91312824619137));
#22980=CARTESIAN_POINT('Ctrl Pts',(12.3486266441811,1.89941801152032,3.71211754524298));
#22981=CARTESIAN_POINT('Ctrl Pts',(12.3090539075271,3.07967827175917,2.81126078045414));
#22982=CARTESIAN_POINT('Ctrl Pts',(12.2694811708731,3.61365242648782,1.62057176809711));
#22983=CARTESIAN_POINT('Ctrl Pts',(12.2299084342191,4.14762658121646,0.429882755740119));
#22984=CARTESIAN_POINT('Ctrl Pts',(12.1903356975651,4.03531463043501,-1.05063850418497));
#22985=CARTESIAN_POINT('Ctrl Pts',(12.1507629609111,3.32783397082584,-2.14715108281151));
#22986=CARTESIAN_POINT('Ctrl Pts',(12.111190224257,2.62035331121666,-3.24366366143806));
#22987=CARTESIAN_POINT('Ctrl Pts',(12.071617487603,1.31770394277974,-3.95616755876599));
#22988=CARTESIAN_POINT('Ctrl Pts',(12.032044750949,0.0127706062405369,-3.96037544027009));
#22989=CARTESIAN_POINT('Ctrl Pts',(11.992472014295,-1.29216273029871,-3.9645833217742));
#22990=CARTESIAN_POINT('Ctrl Pts',(11.952899277641,-2.59938003494028,-3.26049518745443));
#22991=CARTESIAN_POINT('Ctrl Pts',(11.913326540987,-3.31391752573424,-2.16856804058342));
#22992=CARTESIAN_POINT('Ctrl Pts',(11.8902709755349,-3.73021589880342,-1.53239778974413));
#22993=CARTESIAN_POINT('Ctrl Pts',(11.8672154100828,-3.94533671859644,-0.764580565636778));
#22994=CARTESIAN_POINT('Ctrl Pts',(11.8441598446308,-3.9483118015039,0.00169262224176542));
#22995=CARTESIAN_POINT('Ctrl Pts',(11.7388401553692,-3.94800490926472,0.00129567598274352));
#22996=CARTESIAN_POINT('Ctrl Pts',(11.7610857250527,-3.94581749017334,-0.738200375482764));
#22997=CARTESIAN_POINT('Ctrl Pts',(11.7833312947362,-3.74646900286499,-1.47879122073117));
#22998=CARTESIAN_POINT('Ctrl Pts',(11.8055768644197,-3.35737431122418,-2.10066060696583));
#22999=CARTESIAN_POINT('Ctrl Pts',(11.8451496010737,-2.6652121420887,-3.20690665077582));
#23000=CARTESIAN_POINT('Ctrl Pts',(11.8847223377277,-1.37259810121253,-3.93745863244953));
#23001=CARTESIAN_POINT('Ctrl Pts',(11.9242950743818,-0.0678494752439936,
-3.95981485683605));
#23002=CARTESIAN_POINT('Ctrl Pts',(11.9638678110358,1.23689915072447,-3.98217108122257));
#23003=CARTESIAN_POINT('Ctrl Pts',(12.0034405476898,2.55378236178524,-3.29633154832198));
#23004=CARTESIAN_POINT('Ctrl Pts',(12.0430132843438,3.2834370589297,-2.21444763560813));
#23005=CARTESIAN_POINT('Ctrl Pts',(12.0825860209978,4.01309175607421,-1.13256372289422));
#23006=CARTESIAN_POINT('Ctrl Pts',(12.1221587576518,4.1555179393023,0.345364569633074));
#23007=CARTESIAN_POINT('Ctrl Pts',(12.1617314943058,3.64589209342869,1.54667646725719));
#23008=CARTESIAN_POINT('Ctrl Pts',(12.2013042309598,3.1362662475551,2.74798836488128));
#23009=CARTESIAN_POINT('Ctrl Pts',(12.2408769676139,1.97458837257992,3.67268386760227));
#23010=CARTESIAN_POINT('Ctrl Pts',(12.2804497042679,0.689581779690363,3.89989925801654));
#23011=CARTESIAN_POINT('Ctrl Pts',(12.3200224409219,-0.595424813199232,
4.12711464843081));
#23012=CARTESIAN_POINT('Ctrl Pts',(12.3595951775759,-2.00376012400316,3.65684992653832));
#23013=CARTESIAN_POINT('Ctrl Pts',(12.3991679142299,-2.89443776269302,2.70314026365419));
#23014=CARTESIAN_POINT('Ctrl Pts',(12.4290586612764,-3.56719942258961,1.98276819188519));
#23015=CARTESIAN_POINT('Ctrl Pts',(12.4589494083228,-3.94461989025521,0.986574446948708));
#23016=CARTESIAN_POINT('Ctrl Pts',(12.4888401553692,-3.95353526093205,-0.00355836282268518));
#23017=CARTESIAN_POINT('Origin',(4.7,0.,0.));
#23018=CARTESIAN_POINT('',(13.3441598446308,-3.95992130118435,0.00122964282165419));
#23019=CARTESIAN_POINT('',(13.2388401553692,-3.95951177378463,0.0016722506470103));
#23020=CARTESIAN_POINT('',(4.7,-3.954,-4.84225344382863E-16));
#23021=CARTESIAN_POINT('Ctrl Pts',(13.3441598446308,-3.95992130118435,0.00122964282165419));
#23022=CARTESIAN_POINT('Ctrl Pts',(13.342088249931,-3.96020131501855,0.0695639880146641));
#23023=CARTESIAN_POINT('Ctrl Pts',(13.3400166552312,-3.9585846683956,0.137884811974986));
#23024=CARTESIAN_POINT('Ctrl Pts',(13.3379450605315,-3.95502961063748,0.206104619115586));
#23025=CARTESIAN_POINT('Ctrl Pts',(13.2983723238774,-3.88711895008823,1.50927674195507));
#23026=CARTESIAN_POINT('Ctrl Pts',(13.2587995872234,-3.11186785732278,2.77558708680145));
#23027=CARTESIAN_POINT('Ctrl Pts',(13.2192268505694,-1.9821229161865,3.42869127999069));
#23028=CARTESIAN_POINT('Ctrl Pts',(13.1796541139154,-0.852377975050223,
4.08179547317992));
#23029=CARTESIAN_POINT('Ctrl Pts',(13.1400813772614,0.63186081445685,4.12169351471201));
#23030=CARTESIAN_POINT('Ctrl Pts',(13.1005086406074,1.7950608697933,3.53022572037632));
#23031=CARTESIAN_POINT('Ctrl Pts',(13.0609359039534,2.95826092512974,2.93875792604063));
#23032=CARTESIAN_POINT('Ctrl Pts',(13.0213631672994,3.80042224629552,1.71592429583719));
#23033=CARTESIAN_POINT('Ctrl Pts',(12.9817904306453,3.93824535103146,0.418282733106529));
#23034=CARTESIAN_POINT('Ctrl Pts',(12.9422176939913,4.07606845576739,-0.879358829624127));
#23035=CARTESIAN_POINT('Ctrl Pts',(12.9026449573373,3.50955334407346,-2.25180832488194));
#23036=CARTESIAN_POINT('Ctrl Pts',(12.8630722206833,2.49654245255791,-3.07441250840861));
#23037=CARTESIAN_POINT('Ctrl Pts',(12.8234994840293,1.48353156104236,-3.89701669193528));
#23038=CARTESIAN_POINT('Ctrl Pts',(12.7839267473753,0.024024889705067,-4.1697755637308));
#23039=CARTESIAN_POINT('Ctrl Pts',(12.7443540107213,-1.21770120819094,-3.76854621331596));
#23040=CARTESIAN_POINT('Ctrl Pts',(12.7047812740673,-2.45942730608694,-3.36731686290113));
#23041=CARTESIAN_POINT('Ctrl Pts',(12.6652085374132,-3.48337283054174,-2.29209929027598));
#23042=CARTESIAN_POINT('Ctrl Pts',(12.6256358007592,-3.82350162005966,-1.03226551412899));
#23043=CARTESIAN_POINT('Ctrl Pts',(12.6151438153831,-3.91368053077872,-0.698243693215093));
#23044=CARTESIAN_POINT('Ctrl Pts',(12.6046518300069,-3.95579068268866,-0.351244313686516));
#23045=CARTESIAN_POINT('Ctrl Pts',(12.5941598446308,-3.95274743352102,-0.003520024949899));
#23046=CARTESIAN_POINT('Ctrl Pts',(12.4888401553692,-3.95353526093205,-0.00355836282268518));
#23047=CARTESIAN_POINT('Ctrl Pts',(12.4985221449768,-3.95642306183267,-0.324274856104691));
#23048=CARTESIAN_POINT('Ctrl Pts',(12.5082041345844,-3.92064753909048,-0.64435543987071));
#23049=CARTESIAN_POINT('Ctrl Pts',(12.5178861241919,-3.84372223884785,-0.954220416301001));
#23050=CARTESIAN_POINT('Ctrl Pts',(12.557458860846,-3.52930910973709,-2.22071682949655));
#23051=CARTESIAN_POINT('Ctrl Pts',(12.5970315975,-2.52746288493975,-3.316555052012));
#23052=CARTESIAN_POINT('Ctrl Pts',(12.636604334154,-1.29416147990325,-3.7429778691348));
#23053=CARTESIAN_POINT('Ctrl Pts',(12.676177070808,-0.0608600748667443,
-4.1694006862576));
#23054=CARTESIAN_POINT('Ctrl Pts',(12.715749807462,1.40389651040895,-3.92640809798775));
#23055=CARTESIAN_POINT('Ctrl Pts',(12.755322544116,2.43344244506891,-3.12459518761852));
#23056=CARTESIAN_POINT('Ctrl Pts',(12.79489528077,3.46298837972893,-2.32278227724925));
#23057=CARTESIAN_POINT('Ctrl Pts',(12.834468017424,4.05732366377315,-0.962149044780607));
#23058=CARTESIAN_POINT('Ctrl Pts',(12.8740407540781,3.94594393747885,0.338029155260154));
#23059=CARTESIAN_POINT('Ctrl Pts',(12.9136134907321,3.83456421118455,1.63820735530084));
#23060=CARTESIAN_POINT('Ctrl Pts',(12.9531862273861,3.01746947455173,2.87793052291361));
#23061=CARTESIAN_POINT('Ctrl Pts',(12.9927589640401,1.86655030411764,3.4929539495523));
#23062=CARTESIAN_POINT('Ctrl Pts',(13.0323317006941,0.715631133683578,4.10797737619097));
#23063=CARTESIAN_POINT('Ctrl Pts',(13.0719044373481,-0.769112470551771,
4.09830106185561));
#23064=CARTESIAN_POINT('Ctrl Pts',(13.1114771740021,-1.91191786172387,3.46832915347659));
#23065=CARTESIAN_POINT('Ctrl Pts',(13.1510499106561,-3.05472325289603,2.83835724509754));
#23066=CARTESIAN_POINT('Ctrl Pts',(13.1906226473102,-3.85559043100492,1.58808974267472));
#23067=CARTESIAN_POINT('Ctrl Pts',(13.2301953839642,-3.95001454631996,0.286570254467792));
#23068=CARTESIAN_POINT('Ctrl Pts',(13.2330769744325,-3.95689028082004,0.191796769773386));
#23069=CARTESIAN_POINT('Ctrl Pts',(13.2359585649009,-3.96002017282103,0.0967515266364028));
#23070=CARTESIAN_POINT('Ctrl Pts',(13.2388401553692,-3.95951177378463,0.0016722506470103));
#23071=CARTESIAN_POINT('Origin',(4.7,0.,0.));
#23072=CARTESIAN_POINT('',(14.0941598446308,-3.94932298134531,0.002498291375507));
#23073=CARTESIAN_POINT('',(13.9888401553692,-3.94884092925267,0.00217675990483683));
#23074=CARTESIAN_POINT('',(4.7,-3.954,-4.84225344382863E-16));
#23075=CARTESIAN_POINT('Ctrl Pts',(14.0941598446308,-3.94932298134531,0.002498291375507));
#23076=CARTESIAN_POINT('Ctrl Pts',(14.0795246698551,-3.95217299008822,0.488608263067992));
#23077=CARTESIAN_POINT('Ctrl Pts',(14.0648894950794,-3.86903917261975,0.973780078148339));
#23078=CARTESIAN_POINT('Ctrl Pts',(14.0502543203037,-3.69550476445004,1.4241105383856));
#23079=CARTESIAN_POINT('Ctrl Pts',(14.0106815836497,-3.22627692534584,2.64178022688495));
#23080=CARTESIAN_POINT('Ctrl Pts',(13.9711088469957,-2.09610060077861,3.60471329766544));
#23081=CARTESIAN_POINT('Ctrl Pts',(13.9315361103417,-0.819391906539967,
3.87469523990012));
#23082=CARTESIAN_POINT('Ctrl Pts',(13.8919633736876,0.457316787698675,4.14467718213481));
#23083=CARTESIAN_POINT('Ctrl Pts',(13.8523906370336,1.88055785160873,3.72170799582369));
#23084=CARTESIAN_POINT('Ctrl Pts',(13.8128179003796,2.80257668230365,2.7982692338459));
#23085=CARTESIAN_POINT('Ctrl Pts',(13.7732451637256,3.72459551299857,1.87483047186812));
#23086=CARTESIAN_POINT('Ctrl Pts',(13.7336724270716,4.14539211047836,0.450922134223676));
#23087=CARTESIAN_POINT('Ctrl Pts',(13.6940996904176,3.87343771936786,-0.825366984455388));
#23088=CARTESIAN_POINT('Ctrl Pts',(13.6545269537636,3.60148332825735,-2.10165610313449));
#23089=CARTESIAN_POINT('Ctrl Pts',(13.6149542171096,2.63677794855649,-3.2303260028482));
#23090=CARTESIAN_POINT('Ctrl Pts',(13.5753814804555,1.41839970925465,-3.69768418650959));
#23091=CARTESIAN_POINT('Ctrl Pts',(13.5358087438015,0.200021469952839,-4.16504237017096));
#23092=CARTESIAN_POINT('Ctrl Pts',(13.4962360071475,-1.27202962894994,-3.97108883778006));
#23093=CARTESIAN_POINT('Ctrl Pts',(13.4566632704935,-2.32777006423482,-3.20409512116832));
#23094=CARTESIAN_POINT('Ctrl Pts',(13.4191621285393,-3.328243503224,-2.4772527878683));
#23095=CARTESIAN_POINT('Ctrl Pts',(13.381660986585,-3.95485233738253,-1.23579610343927));
#23096=CARTESIAN_POINT('Ctrl Pts',(13.3441598446308,-3.95992130118435,0.00122964282165419));
#23097=CARTESIAN_POINT('Ctrl Pts',(13.2388401553692,-3.95951177378463,0.0016722506470103));
#23098=CARTESIAN_POINT('Ctrl Pts',(13.2755313015549,-3.95303835448019,-1.20896737801102));
#23099=CARTESIAN_POINT('Ctrl Pts',(13.3122224477405,-3.35669606630255,-2.42512468514771));
#23100=CARTESIAN_POINT('Ctrl Pts',(13.3489135939262,-2.39251067506772,-3.15604663613086));
#23101=CARTESIAN_POINT('Ctrl Pts',(13.3884863305802,-1.35260163597929,-3.9443725645315));
#23102=CARTESIAN_POINT('Ctrl Pts',(13.4280590672342,0.115197494718774,-4.16825294734179));
#23103=CARTESIAN_POINT('Ctrl Pts',(13.4676318038883,1.3428363327277,-3.72579203267733));
#23104=CARTESIAN_POINT('Ctrl Pts',(13.5072045405423,2.57047517073663,-3.28333111801288));
#23105=CARTESIAN_POINT('Ctrl Pts',(13.5467772771963,3.55795371605642,-2.17452890587367));
#23106=CARTESIAN_POINT('Ctrl Pts',(13.5863500138503,3.85583289315453,-0.90404179728785));
#23107=CARTESIAN_POINT('Ctrl Pts',(13.6259227505043,4.15371207025265,0.366445311297973));
#23108=CARTESIAN_POINT('Ctrl Pts',(13.6654954871583,3.7619918791291,1.79861731633042));
#23109=CARTESIAN_POINT('Ctrl Pts',(13.7050682238123,2.85895974354046,2.74063655681762));
#23110=CARTESIAN_POINT('Ctrl Pts',(13.7446409604664,1.9559276079518,3.68265579730486));
#23111=CARTESIAN_POINT('Ctrl Pts',(13.7842136971204,0.541583527898016,4.13452227324683));
#23112=CARTESIAN_POINT('Ctrl Pts',(13.8237864337744,-0.74035285927286,3.89057891177458));
#23113=CARTESIAN_POINT('Ctrl Pts',(13.8633591704284,-2.0222892464437,3.64663555030234));
#23114=CARTESIAN_POINT('Ctrl Pts',(13.9029319070824,-3.17181794073164,2.70688235141592));
#23115=CARTESIAN_POINT('Ctrl Pts',(13.9425046437364,-3.66574219400503,1.4990280587802));
#23116=CARTESIAN_POINT('Ctrl Pts',(13.9579498142807,-3.85851997418385,1.0276046213389));
#23117=CARTESIAN_POINT('Ctrl Pts',(13.973394984825,-3.95142773522678,0.515340610393162));
#23118=CARTESIAN_POINT('Ctrl Pts',(13.9888401553692,-3.94884092925267,0.00217675990483683));
#23119=CARTESIAN_POINT('Origin',(4.7,0.,0.));
#23120=CARTESIAN_POINT('',(14.8441598446308,-3.95012252210193,-0.00484157028959653));
#23121=CARTESIAN_POINT('',(14.7388401553692,-3.95165589089271,-0.00363582964324092));
#23122=CARTESIAN_POINT('',(4.7,-3.954,-4.84225344382863E-16));
#23123=CARTESIAN_POINT('Ctrl Pts',(14.8441598446308,-3.95012252210193,-0.00484157028959653));
#23124=CARTESIAN_POINT('Ctrl Pts',(14.8169610897792,-3.94332577709582,0.897842123970638));
#23125=CARTESIAN_POINT('Ctrl Pts',(14.7897623349275,-3.63714466198666,1.80607102634386));
#23126=CARTESIAN_POINT('Ctrl Pts',(14.7625635800759,-3.07096454601399,2.50195343740126));
#23127=CARTESIAN_POINT('Ctrl Pts',(14.7229908434219,-2.24720269550416,3.51442520477352));
#23128=CARTESIAN_POINT('Ctrl Pts',(14.6834181067679,-0.873056840637845,
4.07738712090295));
#23129=CARTESIAN_POINT('Ctrl Pts',(14.6438453701139,0.424568275462648,3.93721918519319));
#23130=CARTESIAN_POINT('Ctrl Pts',(14.6042726334599,1.72219339156307,3.79705124948343));
#23131=CARTESIAN_POINT('Ctrl Pts',(14.5646998968058,2.94329776889771,2.95375346193458));
#23132=CARTESIAN_POINT('Ctrl Pts',(14.5251271601518,3.53287076796465,1.78982106701354));
#23133=CARTESIAN_POINT('Ctrl Pts',(14.4855544234978,4.12244376703158,0.625888672092527));
#23134=CARTESIAN_POINT('Ctrl Pts',(14.4459816868438,4.08048538783091,-0.85867833020057));
#23135=CARTESIAN_POINT('Ctrl Pts',(14.4064089501898,3.425694963339,-1.98750853586906));
#23136=CARTESIAN_POINT('Ctrl Pts',(14.3668362135358,2.77090453884704,-3.11633874153765));
#23137=CARTESIAN_POINT('Ctrl Pts',(14.3272634768818,1.5032820690637,-3.88943215058149));
#23138=CARTESIAN_POINT('Ctrl Pts',(14.2876907402278,0.199979015819173,-3.95528655559086));
#23139=CARTESIAN_POINT('Ctrl Pts',(14.2481180035737,-1.10332403742528,-4.02114096060022));
#23140=CARTESIAN_POINT('Ctrl Pts',(14.2085452669197,-2.44230767413093,-3.37975636157519));
#23141=CARTESIAN_POINT('Ctrl Pts',(14.1689725302657,-3.20765981566317,-2.32286090895358));
#23142=CARTESIAN_POINT('Ctrl Pts',(14.1440349683874,-3.68996197623994,-1.65683682325276));
#23143=CARTESIAN_POINT('Ctrl Pts',(14.1190974065091,-3.94446671755144,-0.825807327419405));
#23144=CARTESIAN_POINT('Ctrl Pts',(14.0941598446308,-3.94932298134531,0.002498291375507));
#23145=CARTESIAN_POINT('Ctrl Pts',(13.9888401553692,-3.94884092925267,0.00217675990483683));
#23146=CARTESIAN_POINT('Ctrl Pts',(14.012967721479,-3.94479996823029,-0.799458592213253));
#23147=CARTESIAN_POINT('Ctrl Pts',(14.0370952875887,-3.70772447792752,-1.60328981463878));
#23148=CARTESIAN_POINT('Ctrl Pts',(14.0612228536984,-3.25429404769414,-2.25705948968798));
#23149=CARTESIAN_POINT('Ctrl Pts',(14.1007955903525,-2.51060183585106,-3.32933735913542));
#23150=CARTESIAN_POINT('Ctrl Pts',(14.1403683270065,-1.18489759990609,-3.99793771164533));
#23151=CARTESIAN_POINT('Ctrl Pts',(14.1799410636605,0.119451583199217,-3.95858537939921));
#23152=CARTESIAN_POINT('Ctrl Pts',(14.2195138003145,1.42380076630463,-3.91923304715309));
#23153=CARTESIAN_POINT('Ctrl Pts',(14.2590865369685,2.70679489657038,-3.1719280301508));
#23154=CARTESIAN_POINT('Ctrl Pts',(14.2986592736225,3.3844745259588,-2.05673988602559));
#23155=CARTESIAN_POINT('Ctrl Pts',(14.3382320102765,4.06215415534718,-0.941551741900444));
#23156=CARTESIAN_POINT('Ctrl Pts',(14.3778047469306,4.1345192838583,0.541519529347578));
#23157=CARTESIAN_POINT('Ctrl Pts',(14.4173774835846,3.56867289191554,1.71736384111271));
#23158=CARTESIAN_POINT('Ctrl Pts',(14.4569502202386,3.00282649997279,2.89320815287784));
#23159=CARTESIAN_POINT('Ctrl Pts',(14.4965229568926,1.79876858757616,3.76182550516009));
#23160=CARTESIAN_POINT('Ctrl Pts',(14.5360956935466,0.504436900763993,3.92808191777024));
#23161=CARTESIAN_POINT('Ctrl Pts',(14.5756684302006,-0.789894786048174,
4.09433833038039));
#23162=CARTESIAN_POINT('Ctrl Pts',(14.6152411668546,-2.17450024727588,3.55823380331844));
#23163=CARTESIAN_POINT('Ctrl Pts',(14.6548139035086,-3.01905207823151,2.56337686971723));
#23164=CARTESIAN_POINT('Ctrl Pts',(14.6828226541288,-3.61680809965312,1.85923805820075));
#23165=CARTESIAN_POINT('Ctrl Pts',(14.710831404749,-3.94402368019253,0.925286740362676));
#23166=CARTESIAN_POINT('Ctrl Pts',(14.7388401553692,-3.95165589089271,-0.00363582964324092));
#23167=CARTESIAN_POINT('Origin',(-7.03243520205041,0.,0.));
#23168=CARTESIAN_POINT('',(14.3425647979496,-3.51958190579553,0.00222644264931085));
#23169=CARTESIAN_POINT('',(14.4904352020504,-3.52166096245149,-0.00324020098756483));
#23170=CARTESIAN_POINT('',(-7.03243520205041,-3.52375,3.2169090177286E-13));
#23171=CARTESIAN_POINT('',(15.,-2.52120044613813,2.46936361140965));
#23172=CARTESIAN_POINT('Ctrl Pts',(14.3425647979496,-3.51958190579553,0.00222644264931099));
#23173=CARTESIAN_POINT('Ctrl Pts',(14.3675023598279,-3.5152540708073,-0.735948045016053));
#23174=CARTESIAN_POINT('Ctrl Pts',(14.4320126583603,-2.92852262828258,-2.65179107551659));
#23175=CARTESIAN_POINT('Ctrl Pts',(14.5360956935466,0.210016568782032,-4.155178159011));
#23176=CARTESIAN_POINT('Ctrl Pts',(14.6548139035087,3.59907929859906,-2.08826776438434));
#23177=CARTESIAN_POINT('Ctrl Pts',(14.7735321134707,3.7112574766783,1.88080884739934));
#23178=CARTESIAN_POINT('Ctrl Pts',(14.8885941456345,0.547106722347347,4.06597940294392));
#23179=CARTESIAN_POINT('Ctrl Pts',(14.9640834411443,-1.7769695191295,3.21936428498554));
#23180=CARTESIAN_POINT('Ctrl Pts',(15.,-2.52120044613813,2.46936361140965));
#23181=CARTESIAN_POINT('',(15.,1.51195443948857,3.18289299779474));
#23182=CARTESIAN_POINT('Origin',(15.,0.,0.));
#23183=CARTESIAN_POINT('Ctrl Pts',(14.4904352020504,-3.52166096245149,-0.00324020098756532));
#23184=CARTESIAN_POINT('Ctrl Pts',(14.5019991880842,-3.52446919194943,-0.345032096527443));
#23185=CARTESIAN_POINT('Ctrl Pts',(14.553135910772,-3.32220045815802,-1.85308063959033));
#23186=CARTESIAN_POINT('Ctrl Pts',(14.6438453701139,-1.17267268992146,-3.99072892597622));
#23187=CARTESIAN_POINT('Ctrl Pts',(14.7625635800759,2.70983253704952,-3.16081271422384));
#23188=CARTESIAN_POINT('Ctrl Pts',(14.881281790038,4.12213179013054,0.556374543543842));
#23189=CARTESIAN_POINT('Ctrl Pts',(14.960427263346,2.56715916810242,2.68164414176901));
#23190=CARTESIAN_POINT('Ctrl Pts',(15.,1.51195443948848,3.18289299779479));
#23191=CARTESIAN_POINT('Origin',(-7.03243520205041,0.,0.));
#23192=CARTESIAN_POINT('',(13.5925647979496,-3.52902698154992,0.00109584064080212));
#23193=CARTESIAN_POINT('',(13.7404352020504,-3.51915230765151,0.00193989825877733));
#23194=CARTESIAN_POINT('',(-7.03243520205041,-3.52375,3.2169090177286E-13));
#23195=CARTESIAN_POINT('Ctrl Pts',(13.5925647979496,-3.52902698154992,0.00109584064080225));
#23196=CARTESIAN_POINT('Ctrl Pts',(13.6300659399038,-3.52450959126252,-1.10132436001352));
#23197=CARTESIAN_POINT('Ctrl Pts',(13.7071398185121,-2.37681150026024,-3.37517909858378));
#23198=CARTESIAN_POINT('Ctrl Pts',(13.8237864337744,1.49012789947011,-3.88467673536986));
#23199=CARTESIAN_POINT('Ctrl Pts',(13.9425046437364,4.06932409197459,-0.867111819500367));
#23200=CARTESIAN_POINT('Ctrl Pts',(14.0612228536985,2.9442998048962,2.93979030855331));
#23201=CARTESIAN_POINT('Ctrl Pts',(14.1799410636605,-0.860818327845137,
4.07062313879903));
#23202=CARTESIAN_POINT('Ctrl Pts',(14.2737217117442,-3.2477048593109,2.03694757208693));
#23203=CARTESIAN_POINT('Ctrl Pts',(14.3279296231739,-3.52212179408783,0.435440912237356));
#23204=CARTESIAN_POINT('Ctrl Pts',(14.3425647979496,-3.51958190579553,0.00222644264931099));
#23205=CARTESIAN_POINT('Ctrl Pts',(13.7404352020504,-3.51915230765151,0.00193989825877757));
#23206=CARTESIAN_POINT('Ctrl Pts',(13.7645627681601,-3.51555105919362,-0.712466417377603));
#23207=CARTESIAN_POINT('Ctrl Pts',(13.8282630709239,-2.95774521056077,-2.60377013928517));
#23208=CARTESIAN_POINT('Ctrl Pts',(13.9315361103417,0.125484922544878,-4.15875404743734));
#23209=CARTESIAN_POINT('Ctrl Pts',(14.0502543203037,3.55564468470245,-2.16079042553925));
#23210=CARTESIAN_POINT('Ctrl Pts',(14.1689725302657,3.74911708348173,1.80428726191164));
#23211=CARTESIAN_POINT('Ctrl Pts',(14.2876907402278,0.529997911397081,4.12658649947203));
#23212=CARTESIAN_POINT('Ctrl Pts',(14.394844964156,-2.81124210751884,2.83289385539345));
#23213=CARTESIAN_POINT('Ctrl Pts',(14.4624264514302,-3.51485924205318,0.824602719108089));
#23214=CARTESIAN_POINT('Ctrl Pts',(14.4904352020504,-3.52166096245149,-0.00324020098756532));
#23215=CARTESIAN_POINT('Origin',(-7.03243520205041,0.,0.));
#23216=CARTESIAN_POINT('',(12.8425647979496,-3.52263373011373,-0.00313699744994253));
#23217=CARTESIAN_POINT('',(12.9904352020504,-3.52866201640708,0.00149028660038811));
#23218=CARTESIAN_POINT('',(-7.03243520205041,-3.52375,3.2169090177286E-13));
#23219=CARTESIAN_POINT('Ctrl Pts',(12.8425647979496,-3.52263373011373,-0.00313699744994185));
#23220=CARTESIAN_POINT('Ctrl Pts',(12.8530567833258,-3.52534583159438,-0.313024064327951));
#23221=CARTESIAN_POINT('Ctrl Pts',(12.9031215053559,-3.34627313867605,-1.78863292620238));
#23222=CARTESIAN_POINT('Ctrl Pts',(12.9927589640401,-1.2792814688989,-3.95912511815523));
#23223=CARTESIAN_POINT('Ctrl Pts',(13.1114771740022,2.62279488400284,-3.22988833933176));
#23224=CARTESIAN_POINT('Ctrl Pts',(13.2301953839642,4.1374061319782,0.439435567280381));
#23225=CARTESIAN_POINT('Ctrl Pts',(13.3489135939262,1.88583863921803,3.70875271783386));
#23226=CARTESIAN_POINT('Ctrl Pts',(13.4676318038883,-2.08236047650701,3.60208297288041));
#23227=CARTESIAN_POINT('Ctrl Pts',(13.5488488718961,-3.50031412078277,1.28596967099022));
#23228=CARTESIAN_POINT('Ctrl Pts',(13.5904932032498,-3.52927652599813,0.0619944620048905));
#23229=CARTESIAN_POINT('Ctrl Pts',(13.5925647979496,-3.52902698154992,0.00109584064080225));
#23230=CARTESIAN_POINT('Ctrl Pts',(12.9904352020504,-3.52866201640708,0.00149028660038825));
#23231=CARTESIAN_POINT('Ctrl Pts',(13.0271263482361,-3.5228929948406,-1.07741497174151));
#23232=CARTESIAN_POINT('Ctrl Pts',(13.1033902310757,-2.41825070574393,-3.33017956397349));
#23233=CARTESIAN_POINT('Ctrl Pts',(13.2192268505694,1.41074465321508,-3.91420835157396));
#23234=CARTESIAN_POINT('Ctrl Pts',(13.3379450605315,4.05082623445229,-0.949760859141879));
#23235=CARTESIAN_POINT('Ctrl Pts',(13.4566632704935,3.00353941846475,2.8792346664523));
#23236=CARTESIAN_POINT('Ctrl Pts',(13.5753814804555,-0.777792108158467,
4.08732608875924));
#23237=CARTESIAN_POINT('Ctrl Pts',(13.6699721243078,-3.2265189232229,2.08546317825473));
#23238=CARTESIAN_POINT('Ctrl Pts',(13.7249900315061,-3.52145763328409,0.459264409679643));
#23239=CARTESIAN_POINT('Ctrl Pts',(13.7404352020504,-3.51915230765151,0.00193989825877757));
#23240=CARTESIAN_POINT('Origin',(-7.03243520205041,0.,0.));
#23241=CARTESIAN_POINT('',(12.0925647979496,-3.5186807563352,0.00150844148329803));
#23242=CARTESIAN_POINT('',(12.2404352020504,-3.52333583098364,-0.00317116363052899));
#23243=CARTESIAN_POINT('',(-7.03243520205041,-3.52375,3.2169090177286E-13));
#23244=CARTESIAN_POINT('Ctrl Pts',(12.0925647979496,-3.5186807563352,0.00150844148329801));
#23245=CARTESIAN_POINT('Ctrl Pts',(12.1156203634017,-3.51602940368091,-0.68138360348061));
#23246=CARTESIAN_POINT('Ctrl Pts',(12.1782486655078,-2.99525967935504,-2.54013425586182));
#23247=CARTESIAN_POINT('Ctrl Pts',(12.2804497042679,0.0134164280071953,
-4.16065529676554));
#23248=CARTESIAN_POINT('Ctrl Pts',(12.3991679142299,3.49612561771096,-2.25573450146264));
#23249=CARTESIAN_POINT('Ctrl Pts',(12.5178861241919,3.79639817959729,1.70252558174023));
#23250=CARTESIAN_POINT('Ctrl Pts',(12.636604334154,0.640903420859428,4.11101877212304));
#23251=CARTESIAN_POINT('Ctrl Pts',(12.7448305587399,-2.76755685483373,2.89521893475459));
#23252=CARTESIAN_POINT('Ctrl Pts',(12.8134840466717,-3.51511656860697,0.855780394542055));
#23253=CARTESIAN_POINT('Ctrl Pts',(12.8425647979496,-3.52263373011373,-0.00313699744994185));
#23254=CARTESIAN_POINT('Ctrl Pts',(12.2404352020504,-3.52333583098364,-0.00317116363052868));
#23255=CARTESIAN_POINT('Ctrl Pts',(12.250117191658,-3.52590939912316,-0.28898925751087));
#23256=CARTESIAN_POINT('Ctrl Pts',(12.2993719179196,-3.36371430659345,-1.74013506675719));
#23257=CARTESIAN_POINT('Ctrl Pts',(12.3881993808351,-1.35960842341351,-3.93226373321093));
#23258=CARTESIAN_POINT('Ctrl Pts',(12.5069175907972,2.55650388111248,-3.28260885239469));
#23259=CARTESIAN_POINT('Ctrl Pts',(12.6256358007592,4.14549398517236,0.355123585322626));
#23260=CARTESIAN_POINT('Ctrl Pts',(12.7443540107213,1.96094347059736,3.66959590085791));
#23261=CARTESIAN_POINT('Ctrl Pts',(12.8630722206833,-2.008605296796,3.64372570917414));
#23262=CARTESIAN_POINT('Ctrl Pts',(12.9450992844597,-3.48802023705692,1.33414869944489));
#23263=CARTESIAN_POINT('Ctrl Pts',(12.987553611582,-3.52911509458222,0.0862236196220098));
#23264=CARTESIAN_POINT('Ctrl Pts',(12.9904352020504,-3.52866201640708,0.00149028660038825));
#23265=CARTESIAN_POINT('Origin',(-7.03243520205041,0.,0.));
#23266=CARTESIAN_POINT('',(11.3425647979496,-3.52804248985531,0.00196469682072595));
#23267=CARTESIAN_POINT('',(11.4904352020504,-3.51840725822498,0.00115468847878691));
#23268=CARTESIAN_POINT('',(-7.03243520205041,-3.52375,3.2169090177286E-13));
#23269=CARTESIAN_POINT('Ctrl Pts',(11.3425647979496,-3.52804248985531,0.00196469682072596));
#23270=CARTESIAN_POINT('Ctrl Pts',(11.3781839434776,-3.52101191020695,-1.04590445150779));
#23271=CARTESIAN_POINT('Ctrl Pts',(11.4533758256596,-2.4718083520435,-3.27018269306563));
#23272=CARTESIAN_POINT('Ctrl Pts',(11.5681404444956,1.30478777373567,-3.9507924973221));
#23273=CARTESIAN_POINT('Ctrl Pts',(11.6868586544577,4.02376996992659,-1.05854037242841));
#23274=CARTESIAN_POINT('Ctrl Pts',(11.8055768644197,3.0800139384955,2.79727485773682));
#23275=CARTESIAN_POINT('Ctrl Pts',(11.9242950743818,-0.66740256042652,4.10680000910255));
#23276=CARTESIAN_POINT('Ctrl Pts',(12.0199577188917,-3.19751819588237,2.14968840054265));
#23277=CARTESIAN_POINT('Ctrl Pts',(12.0760476267477,-3.52058020424936,0.490737163396706));
#23278=CARTESIAN_POINT('Ctrl Pts',(12.0925647979496,-3.5186807563352,0.00150844148329801));
#23279=CARTESIAN_POINT('Ctrl Pts',(11.4904352020504,-3.51840725822498,0.00115468847878698));
#23280=CARTESIAN_POINT('Ctrl Pts',(11.5126807717339,-3.51645786064706,-0.657873943628404));
#23281=CARTESIAN_POINT('Ctrl Pts',(11.5744990780714,-3.02276716911119,-2.4919626366133));
#23282=CARTESIAN_POINT('Ctrl Pts',(11.6758901210629,-0.071280686042087,
-4.16006636356011));
#23283=CARTESIAN_POINT('Ctrl Pts',(11.7946083310249,3.44948351348419,-2.32643430433509));
#23284=CARTESIAN_POINT('Ctrl Pts',(11.913326540987,3.83026823514579,1.62489332904317));
#23285=CARTESIAN_POINT('Ctrl Pts',(12.032044750949,0.724454569027592,4.09712077799104));
#23286=CARTESIAN_POINT('Ctrl Pts',(12.1410809713035,-2.73373818088755,2.94237727385996));
#23287=CARTESIAN_POINT('Ctrl Pts',(12.210544455004,-3.51539057619789,0.879221473807933));
#23288=CARTESIAN_POINT('Ctrl Pts',(12.2404352020504,-3.52333583098364,-0.00317116363052868));
#23289=CARTESIAN_POINT('Origin',(-7.03243520205041,0.,0.));
#23290=CARTESIAN_POINT('',(10.5925647979496,-3.52428395044692,-0.00313728131290625));
#23291=CARTESIAN_POINT('',(10.7404352020504,-3.52748926863011,0.00227945981369715));
#23292=CARTESIAN_POINT('',(-7.03243520205041,-3.52375,3.2169090177286E-13));
#23293=CARTESIAN_POINT('Ctrl Pts',(10.5925647979496,-3.52428395044692,-0.00313728131290616));
#23294=CARTESIAN_POINT('Ctrl Pts',(10.6011747868995,-3.5266064408766,-0.25713421757632));
#23295=CARTESIAN_POINT('Ctrl Pts',(10.6493575125034,-3.38590629208833,-1.6759855412164));
#23296=CARTESIAN_POINT('Ctrl Pts',(10.7371129747614,-1.46504644039007,-3.89420998646693));
#23297=CARTESIAN_POINT('Ctrl Pts',(10.8558311847234,2.46714564844276,-3.35028727732022));
#23298=CARTESIAN_POINT('Ctrl Pts',(10.9745493946854,4.1535561077605,0.243319031071492));
#23299=CARTESIAN_POINT('Ctrl Pts',(11.0932676046475,2.05908722991844,3.61543804687332));
#23300=CARTESIAN_POINT('Ctrl Pts',(11.2119858146095,-1.90971779724849,3.69651327957846));
#23301=CARTESIAN_POINT('Ctrl Pts',(11.2950848790436,-3.47095393416288,1.39797660948795));
#23302=CARTESIAN_POINT('Ctrl Pts',(11.3386112068236,-3.52882285774164,0.118274229366946));
#23303=CARTESIAN_POINT('Ctrl Pts',(11.3425647979496,-3.52804248985531,0.00196469682072596));
#23304=CARTESIAN_POINT('Ctrl Pts',(10.7404352020504,-3.52748926863011,0.00227945981369699));
#23305=CARTESIAN_POINT('Ctrl Pts',(10.7752443518098,-3.51977862026482,-1.02218281736217));
#23306=CARTESIAN_POINT('Ctrl Pts',(10.8496262382232,-2.51131260490639,-3.22453425679115));
#23307=CARTESIAN_POINT('Ctrl Pts',(10.9635808612907,1.22409507255686,-3.97653421179419));
#23308=CARTESIAN_POINT('Ctrl Pts',(11.0822990712527,4.00138863696973,-1.14022895073704));
#23309=CARTESIAN_POINT('Ctrl Pts',(11.2010172812148,3.13631714721284,2.73399850699711));
#23310=CARTESIAN_POINT('Ctrl Pts',(11.3197354911768,-0.583666227467498,
4.11953478190202));
#23311=CARTESIAN_POINT('Ctrl Pts',(11.4162081314553,-3.17485254267083,2.19819996255183));
#23312=CARTESIAN_POINT('Ctrl Pts',(11.4731080350799,-3.51992565212565,0.514474837584795));
#23313=CARTESIAN_POINT('Ctrl Pts',(11.4904352020504,-3.51840725822498,0.00115468847878698));
#23314=CARTESIAN_POINT('Origin',(-7.03243520205041,0.,0.));
#23315=CARTESIAN_POINT('',(9.84256479794961,-3.51816102544073,0.000661434852013216));
#23316=CARTESIAN_POINT('',(9.99043520205041,-3.52500134015064,-0.00305115446425308));
#23317=CARTESIAN_POINT('',(-7.03243520205041,-3.52375,3.2169090177286E-13));
#23318=CARTESIAN_POINT('Ctrl Pts',(9.84256479794961,-3.51816102544073,0.000661434852013316));
#23319=CARTESIAN_POINT('Ctrl Pts',(9.86373836697544,-3.5171024289349,-0.626718687907311));
#23320=CARTESIAN_POINT('Ctrl Pts',(9.92448467265527,-3.05808178285527,-2.42809871725697));
#23321=CARTESIAN_POINT('Ctrl Pts',(10.0248037149891,-0.183323073196887,
-4.15663627733209));
#23322=CARTESIAN_POINT('Ctrl Pts',(10.1435219249512,3.3855596180177,-2.41851577709298));
#23323=CARTESIAN_POINT('Ctrl Pts',(10.2622401349132,3.87265117113374,1.52111978421037));
#23324=CARTESIAN_POINT('Ctrl Pts',(10.3809583448753,0.834564199366861,4.07611764898101));
#23325=CARTESIAN_POINT('Ctrl Pts',(10.4910665658874,-2.68777420777237,3.00452075401946));
#23326=CARTESIAN_POINT('Ctrl Pts',(10.5616020502455,-3.51593194376749,0.910271911299991));
#23327=CARTESIAN_POINT('Ctrl Pts',(10.5925647979496,-3.52428395044692,-0.00313728131290616));
#23328=CARTESIAN_POINT('Ctrl Pts',(9.99043520205041,-3.52500134015064,-0.00305115446425291));
#23329=CARTESIAN_POINT('Ctrl Pts',(9.99823519523173,-3.52709205714162,-0.233032594568881));
#23330=CARTESIAN_POINT('Ctrl Pts',(10.0456079250671,-3.40201178448786,-1.62754596340236));
#23331=CARTESIAN_POINT('Ctrl Pts',(10.1325533915564,-1.54401347143674,-3.86358065584526));
#23332=CARTESIAN_POINT('Ctrl Pts',(10.2512716015185,2.3984360100751,-3.39981437578226));
#23333=CARTESIAN_POINT('Ctrl Pts',(10.3699898114805,4.15764854552659,0.158718795611215));
#23334=CARTESIAN_POINT('Ctrl Pts',(10.4887080214425,2.13225649899359,3.57277417516111));
#23335=CARTESIAN_POINT('Ctrl Pts',(10.6074262314046,-1.83407587178631,3.73462163822996));
#23336=CARTESIAN_POINT('Ctrl Pts',(10.6913352916072,-3.45744840424911,1.4462515066276));
#23337=CARTESIAN_POINT('Ctrl Pts',(10.7356716151558,-3.52854446083548,0.142475790700775));
#23338=CARTESIAN_POINT('Ctrl Pts',(10.7404352020504,-3.52748926863011,0.00227945981369699));
#23339=CARTESIAN_POINT('Origin',(-7.03243520205041,0.,0.));
#23340=CARTESIAN_POINT('',(9.09256479794961,-3.52666944689073,0.00262945503923755));
#23341=CARTESIAN_POINT('',(9.24043520205041,-3.51806531536473,0.000276846526976737));
#23342=CARTESIAN_POINT('',(-7.03243520205041,-3.52375,3.2169090177286E-13));
#23343=CARTESIAN_POINT('Ctrl Pts',(9.09256479794961,-3.52666944689073,0.00262945503923759));
#23344=CARTESIAN_POINT('Ctrl Pts',(9.12630194705135,-3.51838375617842,-0.990886089246301));
#23345=CARTESIAN_POINT('Ctrl Pts',(9.19961183280712,-2.56233043718894,-3.16372988524757));
#23346=CARTESIAN_POINT('Ctrl Pts',(9.31249445521691,1.11652672540754,-4.00806693589946));
#23347=CARTESIAN_POINT('Ctrl Pts',(9.43121266517893,3.96921968490559,-1.24760874642564));
#23348=CARTESIAN_POINT('Ctrl Pts',(9.54993087514098,3.20883019120772,2.64851681044191));
#23349=CARTESIAN_POINT('Ctrl Pts',(9.66864908510301,-0.472478016872994,
4.1337630574056));
#23350=CARTESIAN_POINT('Ctrl Pts',(9.76619372603923,-3.14384070009375,2.26236328063938));
#23351=CARTESIAN_POINT('Ctrl Pts',(9.82416563032143,-3.51908091261411,0.545835091270507));
#23352=CARTESIAN_POINT('Ctrl Pts',(9.84256479794961,-3.51816102544073,0.000661434852013316));
#23353=CARTESIAN_POINT('Ctrl Pts',(9.24043520205041,-3.51806531536473,0.000276846526976876));
#23354=CARTESIAN_POINT('Ctrl Pts',(9.26079877530765,-3.51763984226101,-0.60314385718963));
#23355=CARTESIAN_POINT('Ctrl Pts',(9.3207350852189,-3.08395212212633,-2.3797714594065));
#23356=CARTESIAN_POINT('Ctrl Pts',(9.42024413178417,-0.267897613543705,
-4.1520433466978));
#23357=CARTESIAN_POINT('Ctrl Pts',(9.53896234174623,3.33562684382852,-2.48693116972114));
#23358=CARTESIAN_POINT('Ctrl Pts',(9.65768055170824,3.90281273176416,1.44197290715868));
#23359=CARTESIAN_POINT('Ctrl Pts',(9.77639876167031,0.917364772580788,4.05828473104436));
#23360=CARTESIAN_POINT('Ctrl Pts',(9.88731697845101,-2.652123974148,3.05125664466314));
#23361=CARTESIAN_POINT('Ctrl Pts',(9.95866245857771,-3.51648494621486,0.933762651658492));
#23362=CARTESIAN_POINT('Ctrl Pts',(9.99043520205041,-3.52500134015064,-0.00305115446425291));
#23363=CARTESIAN_POINT('Origin',(-7.03243520205041,0.,0.));
#23364=CARTESIAN_POINT('',(8.34256479794962,-3.52593087787563,-0.00285764939352675));
#23365=CARTESIAN_POINT('',(8.49043520205041,-3.52600078018851,0.00283908784911309));
#23366=CARTESIAN_POINT('',(-7.03243520205041,-3.52375,3.2169090177286E-13));
#23367=CARTESIAN_POINT('Ctrl Pts',(8.34256479794962,-3.52593087787563,-0.00285764939352656));
#23368=CARTESIAN_POINT('Ctrl Pts',(8.34929279047327,-3.52767436669035,-0.201096201058421));
#23369=CARTESIAN_POINT('Ctrl Pts',(8.39559351965095,-3.42246428829984,-1.56348475987019));
#23370=CARTESIAN_POINT('Ctrl Pts',(8.48146698548262,-1.64753430101277,-3.82058414619887));
#23371=CARTESIAN_POINT('Ctrl Pts',(8.60018519544467,2.305977735937,-3.46319204962163));
#23372=CARTESIAN_POINT('Ctrl Pts',(8.7189034054067,4.16041530571664,0.0466580663793381));
#23373=CARTESIAN_POINT('Ctrl Pts',(8.83762161536874,2.22772978017945,3.5140364991988));
#23374=CARTESIAN_POINT('Ctrl Pts',(8.95633982533078,-1.73280303479793,3.78267446838806));
#23375=CARTESIAN_POINT('Ctrl Pts',(9.04132088619107,-3.43875275553379,1.51020068927361));
#23376=CARTESIAN_POINT('Ctrl Pts',(9.08672921039734,-3.5281026407103,0.174479984724652));
#23377=CARTESIAN_POINT('Ctrl Pts',(9.09256479794961,-3.52666944689073,0.00262945503923759));
#23378=CARTESIAN_POINT('Ctrl Pts',(8.49043520205041,-3.52600078018851,0.0028390878491133));
#23379=CARTESIAN_POINT('Ctrl Pts',(8.52336235538358,-3.51750136365036,-0.967301129892824));
#23380=CARTESIAN_POINT('Ctrl Pts',(8.59586224537075,-2.59993141150347,-3.11751026790667));
#23381=CARTESIAN_POINT('Ctrl Pts',(8.70793487201195,1.03470715069641,-4.02996454035241));
#23382=CARTESIAN_POINT('Ctrl Pts',(8.82665308197397,3.9430009766923,-1.32814772597166));
#23383=CARTESIAN_POINT('Ctrl Pts',(8.94537129193603,3.26207859074647,2.58264909579165));
#23384=CARTESIAN_POINT('Ctrl Pts',(9.06408950189805,-0.388233209948286,
4.14252435827397));
#23385=CARTESIAN_POINT('Ctrl Pts',(9.16244413860286,-3.11963096819313,2.31080554513191));
#23386=CARTESIAN_POINT('Ctrl Pts',(9.22122603865364,-3.51846666842133,0.569489663367105));
#23387=CARTESIAN_POINT('Ctrl Pts',(9.24043520205041,-3.51806531536473,0.000276846526976876));
#23388=CARTESIAN_POINT('Origin',(-7.03243520205041,0.,0.));
#23389=CARTESIAN_POINT('',(7.59256479794961,-3.51805992519622,-0.000237397935153123));
#23390=CARTESIAN_POINT('',(7.74043520205041,-3.52660313318512,-0.00265300288022408));
#23391=CARTESIAN_POINT('',(-7.03243520205041,-3.52375,3.2169090177286E-13));
#23392=CARTESIAN_POINT('Ctrl Pts',(7.59256479794961,-3.51805992519622,-0.000237397935152622));
#23393=CARTESIAN_POINT('Ctrl Pts',(7.61185637054919,-3.51840553530387,-0.571894346614677));
#23394=CARTESIAN_POINT('Ctrl Pts',(7.67072067980279,-3.11712991020214,-2.31573181407069));
#23395=CARTESIAN_POINT('Ctrl Pts',(7.76915772571038,-0.379652508136737,
-4.14331949821216));
#23396=CARTESIAN_POINT('Ctrl Pts',(7.88787593567244,3.26742063740621,-2.57588720045187));
#23397=CARTESIAN_POINT('Ctrl Pts',(8.00659414563445,3.940241635325,1.33631147059774));
#23398=CARTESIAN_POINT('Ctrl Pts',(8.12531235559652,1.02635818146356,4.03209887955918));
#23399=CARTESIAN_POINT('Ctrl Pts',(8.23730257303488,-2.60371145120387,3.11279511355487));
#23400=CARTESIAN_POINT('Ctrl Pts',(8.30972005381926,-3.51741950634657,0.964904202795411));
#23401=CARTESIAN_POINT('Ctrl Pts',(8.34256479794962,-3.52593087787563,-0.00285764939352656));
#23402=CARTESIAN_POINT('Ctrl Pts',(7.74043520205041,-3.52660313318512,-0.00265300288022373));
#23403=CARTESIAN_POINT('Ctrl Pts',(7.74635319880549,-3.52806540306219,-0.17693892227022));
#23404=CARTESIAN_POINT('Ctrl Pts',(7.79184393221457,-3.43727644157581,-1.51511944087091));
#23405=CARTESIAN_POINT('Ctrl Pts',(7.87690740227768,-1.7249647945704,-3.78625534554826));
#23406=CARTESIAN_POINT('Ctrl Pts',(7.9956256122397,2.2350031991217,-3.50941502021571));
#23407=CARTESIAN_POINT('Ctrl Pts',(8.11434382220176,4.16050309010526,-0.0380410492039316));
#23408=CARTESIAN_POINT('Ctrl Pts',(8.23306203216378,2.2987999778154,3.46796074749932));
#23409=CARTESIAN_POINT('Ctrl Pts',(8.35178024212583,-1.65544386605393,3.81716369711131));
#23410=CARTESIAN_POINT('Ctrl Pts',(8.4375712987547,-3.42399640853641,1.55856250352173));
#23411=CARTESIAN_POINT('Ctrl Pts',(8.48378961872956,-3.52771619057371,0.198639422748347));
#23412=CARTESIAN_POINT('Ctrl Pts',(8.49043520205041,-3.52600078018851,0.0028390878491133));
#23413=CARTESIAN_POINT('Origin',(-7.03243520205041,0.,0.));
#23414=CARTESIAN_POINT('',(6.84256479794961,-3.52507380456061,0.00303947481950978));
#23415=CARTESIAN_POINT('',(6.99043520205041,-3.51814775897504,-0.000622653609956558));
#23416=CARTESIAN_POINT('',(-7.03243520205041,-3.52375,3.2169090177286E-13));
#23417=CARTESIAN_POINT('Ctrl Pts',(6.84256479794961,-3.52507380456061,0.00303947481950992));
#23418=CARTESIAN_POINT('Ctrl Pts',(6.87441995062511,-3.51654838502914,-0.936154325939411));
#23419=CARTESIAN_POINT('Ctrl Pts',(6.94584783995463,-2.6484521526581,-3.05600034132353));
#23420=CARTESIAN_POINT('Ctrl Pts',(7.05684846593816,0.925768177301577,-4.05637594079931));
#23421=CARTESIAN_POINT('Ctrl Pts',(7.1755666759002,3.90579086153378,-1.43388641013115));
#23422=CARTESIAN_POINT('Ctrl Pts',(7.29428488586224,3.33046878081729,2.49383443540284));
#23423=CARTESIAN_POINT('Ctrl Pts',(7.41300309582428,-0.276496612222895,
4.15147950911829));
#23424=CARTESIAN_POINT('Ctrl Pts',(7.51242973318673,-3.08654526745354,2.37485148050317));
#23425=CARTESIAN_POINT('Ctrl Pts',(7.57228363389518,-3.51769658647637,0.600743589964055));
#23426=CARTESIAN_POINT('Ctrl Pts',(7.59256479794961,-3.51805992519622,-0.000237397935152622));
#23427=CARTESIAN_POINT('Ctrl Pts',(6.99043520205041,-3.51814775897504,-0.000622653609956524));
#23428=CARTESIAN_POINT('Ctrl Pts',(7.00891677888141,-3.5190174026022,-0.548243313944348));
#23429=CARTESIAN_POINT('Ctrl Pts',(7.06697109236642,-3.1414084095468,-2.26729354051509));
#23430=CARTESIAN_POINT('Ctrl Pts',(7.16459814250543,-0.463915294938845,
-4.13473284304098));
#23431=CARTESIAN_POINT('Ctrl Pts',(7.28331635246748,3.21430888617722,-2.64186514955669));
#23432=CARTESIAN_POINT('Ctrl Pts',(7.40203456242951,3.96662723246049,1.25582701153581));
#23433=CARTESIAN_POINT('Ctrl Pts',(7.52075277239156,1.1082229708534,4.01037092188151));
#23434=CARTESIAN_POINT('Ctrl Pts',(7.63355298559851,-2.5661931577787,3.15903810143261));
#23435=CARTESIAN_POINT('Ctrl Pts',(7.70678046215147,-3.51828742866349,0.988484290341461));
#23436=CARTESIAN_POINT('Ctrl Pts',(7.74043520205041,-3.52660313318512,-0.00265300288022373));
#23437=CARTESIAN_POINT('Origin',(-7.03243520205041,0.,0.));
#23438=CARTESIAN_POINT('',(6.09256479794961,-3.52742942371994,-0.00230914916092352));
#23439=CARTESIAN_POINT('',(6.24043520205041,-3.52435719309002,0.00313090232885352));
#23440=CARTESIAN_POINT('',(-7.03243520205041,-3.52375,3.2169090177286E-13));
#23441=CARTESIAN_POINT('Ctrl Pts',(6.09256479794962,-3.52742942371994,-0.00230914916092399));
#23442=CARTESIAN_POINT('Ctrl Pts',(6.09741079404703,-3.52851335812002,-0.144937184098135));
#23443=CARTESIAN_POINT('Ctrl Pts',(6.14182952679845,-3.45604450642565,-1.45116517618719));
#23444=CARTESIAN_POINT('Ctrl Pts',(6.22582099620389,-1.82633687898537,-3.73841224260482));
#23445=CARTESIAN_POINT('Ctrl Pts',(6.34453920616593,2.13965170336266,-3.56835019014346));
#23446=CARTESIAN_POINT('Ctrl Pts',(6.46325741612797,4.15796828993553,-0.15010726528171));
#23447=CARTESIAN_POINT('Ctrl Pts',(6.58197562609,2.39138923910093,3.40477458847308));
#23448=CARTESIAN_POINT('Ctrl Pts',(6.70069383605204,-1.55201225656202,3.86037439203516));
#23449=CARTESIAN_POINT('Ctrl Pts',(6.78755689333858,-3.40361868355192,1.62261932332329));
#23450=CARTESIAN_POINT('Ctrl Pts',(6.8348472139711,-3.52713926762263,0.230579022449037));
#23451=CARTESIAN_POINT('Ctrl Pts',(6.84256479794961,-3.52507380456061,0.00303947481950992));
#23452=CARTESIAN_POINT('Ctrl Pts',(6.24043520205041,-3.52435719309002,0.00313090232885352));
#23453=CARTESIAN_POINT('Ctrl Pts',(6.27148035895733,-3.51598245699914,-0.912660575939013));
#23454=CARTESIAN_POINT('Ctrl Pts',(6.34209825251826,-2.68418353073412,-3.00928463009835));
#23455=CARTESIAN_POINT('Ctrl Pts',(6.45228888273322,0.843004746942437,-4.07438045361901));
#23456=CARTESIAN_POINT('Ctrl Pts',(6.57100709269524,3.87579342533039,-1.51309563754761));
#23457=CARTESIAN_POINT('Ctrl Pts',(6.68972530265728,3.38054326260136,2.42552269292219));
#23458=CARTESIAN_POINT('Ctrl Pts',(6.80844351261932,-0.191931774030066,
4.15624774024814));
#23459=CARTESIAN_POINT('Ctrl Pts',(6.90868014575036,-3.06074569025441,2.42318458251062));
#23460=CARTESIAN_POINT('Ctrl Pts',(6.9693440422274,-3.51715532240443,0.624321580051326));
#23461=CARTESIAN_POINT('Ctrl Pts',(6.99043520205041,-3.51814775897504,-0.000622653609956524));
#23462=CARTESIAN_POINT('Origin',(-7.03243520205041,0.,0.));
#23463=CARTESIAN_POINT('',(5.34256479794961,-3.51838353120525,-0.0011176602703349));
#23464=CARTESIAN_POINT('',(5.49043520205041,-3.52798931335802,-0.00199855428895335));
#23465=CARTESIAN_POINT('',(-7.03243520205041,-3.52375,3.2169090177286E-13));
#23466=CARTESIAN_POINT('Ctrl Pts',(5.34256479794961,-3.51838353120525,-0.00111766027033496));
#23467=CARTESIAN_POINT('Ctrl Pts',(5.35997437412294,-3.51985964985165,-0.516887860646145));
#23468=CARTESIAN_POINT('Ctrl Pts',(5.41695668695029,-3.17250968493244,-2.20313420046544));
#23469=CARTESIAN_POINT('Ctrl Pts',(5.51351173643166,-0.575132718389392,
-4.12073474606626));
#23470=CARTESIAN_POINT('Ctrl Pts',(5.63222994639369,3.14197293576922,-2.72749675748542));
#23471=CARTESIAN_POINT('Ctrl Pts',(5.75094815635573,3.99901838065921,1.14851403228232));
#23472=CARTESIAN_POINT('Ctrl Pts',(5.86966636631777,1.21585635703487,3.97906092065169));
#23473=CARTESIAN_POINT('Ctrl Pts',(5.9835385801824,-2.51528550301645,3.21987535772615));
#23474=CARTESIAN_POINT('Ctrl Pts',(6.05783805739301,-3.51966187543159,1.01977313604934));
#23475=CARTESIAN_POINT('Ctrl Pts',(6.09256479794962,-3.52742942371994,-0.00230914916092399));
#23476=CARTESIAN_POINT('Ctrl Pts',(5.49043520205041,-3.52798931335802,-0.00199855428895362));
#23477=CARTESIAN_POINT('Ctrl Pts',(5.49447120237924,-3.52879682472288,-0.120737180229964));
#23478=CARTESIAN_POINT('Ctrl Pts',(5.53807993936208,-3.46960409793346,-1.40288631934378));
#23479=CARTESIAN_POINT('Ctrl Pts',(5.62126141299893,-1.90205763486351,-3.70046076021046));
#23480=CARTESIAN_POINT('Ctrl Pts',(5.73997962296098,2.06657102730044,-3.61116563914235));
#23481=CARTESIAN_POINT('Ctrl Pts',(5.85869783292301,4.15405122458681,-0.23471580200077));
#23482=CARTESIAN_POINT('Ctrl Pts',(5.97741604288506,2.46020139211735,3.35539002120827));
#23483=CARTESIAN_POINT('Ctrl Pts',(6.09613425284709,-1.47310888518228,3.89116734368968));
#23484=CARTESIAN_POINT('Ctrl Pts',(6.18380730590221,-3.38757081640289,1.67105601217906));
#23485=CARTESIAN_POINT('Ctrl Pts',(6.23190762230332,-3.52665759150933,0.254683338866837));
#23486=CARTESIAN_POINT('Ctrl Pts',(6.24043520205041,-3.52435719309002,0.00313090232885352));
#23487=CARTESIAN_POINT('Origin',(-7.03243520205041,0.,0.));
#23488=CARTESIAN_POINT('',(4.59256479794961,-3.5234081221446,0.00317178002406706));
#23489=CARTESIAN_POINT('',(4.74043520205041,-3.51864963524456,-0.00147337684491794));
#23490=CARTESIAN_POINT('',(-7.03243520205041,-3.52375,3.2169090177286E-13));
#23491=CARTESIAN_POINT('Ctrl Pts',(4.59256479794961,-3.5234081221446,0.00317178002406677));
#23492=CARTESIAN_POINT('Ctrl Pts',(4.62253795419887,-3.51542475237107,-0.88160719352955));
#23493=CARTESIAN_POINT('Ctrl Pts',(4.69208384710213,-2.73025360675707,-2.94716560832423));
#23494=CARTESIAN_POINT('Ctrl Pts',(4.80120247665942,0.732938827149255,-4.09561145213467));
#23495=CARTESIAN_POINT('Ctrl Pts',(4.91992068662146,3.83362538042524,-1.61695668889399));
#23496=CARTESIAN_POINT('Ctrl Pts',(5.0386388965835,3.44465762033206,2.33357373354433));
#23497=CARTESIAN_POINT('Ctrl Pts',(5.15735710654553,-0.0798967268727354,
4.15990973510661));
#23498=CARTESIAN_POINT('Ctrl Pts',(5.25866574033425,-3.02552579319884,2.4870573681738));
#23499=CARTESIAN_POINT('Ctrl Pts',(5.32040163746893,-3.51650436688079,0.655480616923154));
#23500=CARTESIAN_POINT('Ctrl Pts',(5.34256479794961,-3.51838353120525,-0.00111766027033496));
#23501=CARTESIAN_POINT('Ctrl Pts',(4.74043520205041,-3.51864963524456,-0.00147337684491766));
#23502=CARTESIAN_POINT('Ctrl Pts',(4.75703478245516,-3.52051321359516,-0.493153923345435));
#23503=CARTESIAN_POINT('Ctrl Pts',(4.81320709951392,-3.19524209899379,-2.15462497466647));
#23504=CARTESIAN_POINT('Ctrl Pts',(4.90895215322669,-0.658895268659781,
-4.10817357339461));
#23505=CARTESIAN_POINT('Ctrl Pts',(5.02767036318875,3.08580101037766,-2.79088968046971));
#23506=CARTESIAN_POINT('Ctrl Pts',(5.14638857315077,4.02156899374811,1.06687202265491));
#23507=CARTESIAN_POINT('Ctrl Pts',(5.26510678311282,1.29660224356769,3.95348652535647));
#23508=CARTESIAN_POINT('Ctrl Pts',(5.37978899274602,-2.47586534144427,3.2655505474875));
#23509=CARTESIAN_POINT('Ctrl Pts',(5.45489846572523,-3.52087922512356,1.04348779305868));
#23510=CARTESIAN_POINT('Ctrl Pts',(5.49043520205041,-3.52798931335802,-0.00199855428895362));
#23511=CARTESIAN_POINT('Origin',(-7.03243520205041,0.,0.));
#23512=CARTESIAN_POINT('',(3.84256479794961,-3.52861952000803,-0.00152880647882163));
#23513=CARTESIAN_POINT('',(3.99043520205041,-3.52270430891722,0.00314279080041127));
#23514=CARTESIAN_POINT('',(-7.03243520205041,-3.52375,3.2169090177286E-13));
#23515=CARTESIAN_POINT('Ctrl Pts',(3.84256479794961,-3.52861952000803,-0.00152880647882115));
#23516=CARTESIAN_POINT('Ctrl Pts',(3.84552879762077,-3.52909571181233,-0.0886881604188186));
#23517=CARTESIAN_POINT('Ctrl Pts',(3.88806553394595,-3.48674052690646,-1.33905274392585));
#23518=CARTESIAN_POINT('Ctrl Pts',(3.97017500692515,-2.00105422024427,-3.6478780816856));
#23519=CARTESIAN_POINT('Ctrl Pts',(4.08889321688719,1.96853959665618,-3.66552647618271));
#23520=CARTESIAN_POINT('Ctrl Pts',(4.20761142684923,4.14622053401822,-0.346536829911929));
#23521=CARTESIAN_POINT('Ctrl Pts',(4.32632963681127,2.54969952546351,3.28789671690745));
#23522=CARTESIAN_POINT('Ctrl Pts',(4.4450478467733,-1.3677498639029,3.92943924765267));
#23523=CARTESIAN_POINT('Ctrl Pts',(4.53379290048609,-3.36545606309109,1.73520207145909));
#23524=CARTESIAN_POINT('Ctrl Pts',(4.58296521754485,-3.52596497666484,0.286542234120801));
#23525=CARTESIAN_POINT('Ctrl Pts',(4.59256479794961,-3.5234081221446,0.00317178002406677));
#23526=CARTESIAN_POINT('Ctrl Pts',(3.99043520205041,-3.52270430891722,0.0031427908004112));
#23527=CARTESIAN_POINT('Ctrl Pts',(4.01959836253108,-3.51513941180095,-0.858164720925442));
#23528=CARTESIAN_POINT('Ctrl Pts',(4.08833425966577,-2.76415178313285,-2.90002446236997));
#23529=CARTESIAN_POINT('Ctrl Pts',(4.19664289345446,0.649416670297701,-4.10968259997526));
#23530=CARTESIAN_POINT('Ctrl Pts',(4.3153611034165,3.79991631591589,-1.69465898523452));
#23531=CARTESIAN_POINT('Ctrl Pts',(4.43407931337854,3.49144617539216,2.26297076616989));
#23532=CARTESIAN_POINT('Ctrl Pts',(4.55279752334059,0.00479898395836184,
4.16067423069304));
#23533=CARTESIAN_POINT('Ctrl Pts',(4.65491615289787,-2.99809103350652,2.53523688571456));
#23534=CARTESIAN_POINT('Ctrl Pts',(4.71746204580115,-3.51607051724355,0.678992860497283));
#23535=CARTESIAN_POINT('Ctrl Pts',(4.74043520205041,-3.51864963524456,-0.00147337684491766));
#23536=CARTESIAN_POINT('Origin',(-7.03243520205041,0.,0.));
#23537=CARTESIAN_POINT('',(3.09256479794961,-3.51911232364593,-0.00191002701478894));
#23538=CARTESIAN_POINT('',(3.24043520205041,-3.52899431355517,-0.00113694359771377));
#23539=CARTESIAN_POINT('',(-7.03243520205041,-3.52375,3.2169090177286E-13));
#23540=CARTESIAN_POINT('Ctrl Pts',(3.09256479794961,-3.51911232364593,-0.00191002701478871));
#23541=CARTESIAN_POINT('Ctrl Pts',(3.1080923776967,-3.52139001070197,-0.461686364954821));
#23542=CARTESIAN_POINT('Ctrl Pts',(3.1631926940978,-3.22432754532709,-2.09039597570537));
#23543=CARTESIAN_POINT('Ctrl Pts',(3.25786574715292,-0.769326444574681,
-4.08893253953619));
#23544=CARTESIAN_POINT('Ctrl Pts',(3.37658395711495,3.0094971204592,-2.87300532076558));
#23545=CARTESIAN_POINT('Ctrl Pts',(3.495302167077,4.04884993253241,0.958147543456581));
#23546=CARTESIAN_POINT('Ctrl Pts',(3.61402037703903,1.40263484759868,3.9171224100737));
#23547=CARTESIAN_POINT('Ctrl Pts',(3.72977458732991,-2.42241976690523,3.32558458753253));
#23548=CARTESIAN_POINT('Ctrl Pts',(3.80595606096676,-3.52273801445775,1.07498746139492));
#23549=CARTESIAN_POINT('Ctrl Pts',(3.84256479794961,-3.52861952000803,-0.00152880647882115));
#23550=CARTESIAN_POINT('Ctrl Pts',(3.24043520205041,-3.52899431355517,-0.00113694359771367));
#23551=CARTESIAN_POINT('Ctrl Pts',(3.24258920595299,-3.52926239189115,-0.0644596887891739));
#23552=CARTESIAN_POINT('Ctrl Pts',(3.28431594650959,-3.49908651487518,-1.29086897191188));
#23553=CARTESIAN_POINT('Ctrl Pts',(3.3656154237202,-2.07489586267471,-3.60638880921834));
#23554=CARTESIAN_POINT('Ctrl Pts',(3.48433363368223,1.89351625165984,-3.70483863196498));
#23555=CARTESIAN_POINT('Ctrl Pts',(3.60305184364428,4.13830738080923,-0.430865531390001));
#23556=CARTESIAN_POINT('Ctrl Pts',(3.72177005360631,2.6160997115818,3.23531379981317));
#23557=CARTESIAN_POINT('Ctrl Pts',(3.84048826356835,-1.28747878468051,3.95646704310772));
#23558=CARTESIAN_POINT('Ctrl Pts',(3.93004331304971,-3.34807439860695,1.78369783221634));
#23559=CARTESIAN_POINT('Ctrl Pts',(3.98002562587707,-3.52540454344179,0.310580187989291));
#23560=CARTESIAN_POINT('Ctrl Pts',(3.99043520205041,-3.52270430891722,0.0031427908004112));
#23561=CARTESIAN_POINT('Origin',(-7.03243520205041,0.,0.));
#23562=CARTESIAN_POINT('',(2.34256479794961,-3.52180846607991,0.00302771658732861));
#23563=CARTESIAN_POINT('',(2.49043520205041,-3.51954048850984,-0.00220771176014323));
#23564=CARTESIAN_POINT('',(-7.03243520205041,-3.52375,3.2169090177286E-13));
#23565=CARTESIAN_POINT('Ctrl Pts',(2.34256479794961,-3.52180846607991,0.00302771658732888));
#23566=CARTESIAN_POINT('Ctrl Pts',(2.37065595777262,-3.51492881311082,-0.827155541520102));
#23567=CARTESIAN_POINT('Ctrl Pts',(2.43831985424964,-2.80782098383424,-2.83738688689506));
#23568=CARTESIAN_POINT('Ctrl Pts',(2.54555648738068,0.538470004761492,-4.12568570605805));
#23569=CARTESIAN_POINT('Ctrl Pts',(2.66427469734272,3.75288466474145,-1.79641008245562));
#23570=CARTESIAN_POINT('Ctrl Pts',(2.78299290730476,3.55114128675486,2.16809318358432));
#23571=CARTESIAN_POINT('Ctrl Pts',(2.9017111172668,0.116881875255089,4.15903487824236));
#23572=CARTESIAN_POINT('Ctrl Pts',(3.00490174748175,-2.96067738920047,2.59887469195073));
#23573=CARTESIAN_POINT('Ctrl Pts',(3.06851964104268,-3.51558522260769,0.71007434968313));
#23574=CARTESIAN_POINT('Ctrl Pts',(3.09256479794961,-3.51911232364593,-0.00191002701478871));
#23575=CARTESIAN_POINT('Ctrl Pts',(2.49043520205041,-3.51954048850984,-0.00220771176014333));
#23576=CARTESIAN_POINT('Ctrl Pts',(2.50515278602891,-3.52205463920765,-0.437866834869524));
#23577=CARTESIAN_POINT('Ctrl Pts',(2.55944310666143,-3.24555974650898,-2.04185136506832));
#23578=CARTESIAN_POINT('Ctrl Pts',(2.65330616394796,-0.852401394279078,
-4.07242494678922));
#23579=CARTESIAN_POINT('Ctrl Pts',(2.77202437391,2.95039066892461,-2.93367141734082));
#23580=CARTESIAN_POINT('Ctrl Pts',(2.89074258387204,4.06751511929676,0.875530603972367));
#23581=CARTESIAN_POINT('Ctrl Pts',(3.00946079383408,1.48208121505632,3.88775878317795));
#23582=CARTESIAN_POINT('Ctrl Pts',(3.12602499989353,-2.38106696512148,3.37061275541135));
#23583=CARTESIAN_POINT('Ctrl Pts',(3.20301646929898,-3.52433733424402,1.09888746980545));
#23584=CARTESIAN_POINT('Ctrl Pts',(3.24043520205041,-3.52899431355517,-0.00113694359771367));
#23585=CARTESIAN_POINT('Origin',(-7.03243520205041,0.,0.));
#23586=CARTESIAN_POINT('',(1.59256479794961,-3.5293292687682,-0.000582581467793654));
#23587=CARTESIAN_POINT('',(1.74043520205041,-3.52117028029313,0.00288554803045085));
#23588=CARTESIAN_POINT('',(-7.03243520205041,-3.52375,3.2169090177286E-13));
#23589=CARTESIAN_POINT('Ctrl Pts',(1.59256479794961,-3.5293292687682,-0.000582581467793819));
#23590=CARTESIAN_POINT('Ctrl Pts',(1.59364680119453,-3.52940256225382,-0.032382903366644));
#23591=CARTESIAN_POINT('Ctrl Pts',(1.63430154109346,-3.51464154093268,-1.22716522922806));
#23592=CARTESIAN_POINT('Ctrl Pts',(1.71452901764641,-2.17129550877666,-3.54918417453448));
#23593=CARTESIAN_POINT('Ctrl Pts',(1.83324722760845,1.7930241674711,-3.7545035392265));
#23594=CARTESIAN_POINT('Ctrl Pts',(1.95196543757049,4.12519831590081,-0.54219124457039));
#23595=CARTESIAN_POINT('Ctrl Pts',(2.07068364753253,2.70230652333086,3.16366432245317));
#23596=CARTESIAN_POINT('Ctrl Pts',(2.18940185749457,-1.18042802365586,3.98971454770484));
#23597=CARTESIAN_POINT('Ctrl Pts',(2.28002890763359,-3.32416575786672,1.84790964055073));
#23598=CARTESIAN_POINT('Ctrl Pts',(2.33108322111861,-3.52462035653345,0.342344886893788));
#23599=CARTESIAN_POINT('Ctrl Pts',(2.34256479794961,-3.52180846607991,0.00302771658732888));
#23600=CARTESIAN_POINT('Ctrl Pts',(1.74043520205041,-3.52117028029313,0.00288554803045071));
#23601=CARTESIAN_POINT('Ctrl Pts',(1.76771636610483,-3.51488727156751,-0.803729878337304));
#23602=CARTESIAN_POINT('Ctrl Pts',(1.83457026681328,-2.83992472367244,-2.78988645498181));
#23603=CARTESIAN_POINT('Ctrl Pts',(1.94099690417573,0.454375947728439,-4.13579201391049));
#23604=CARTESIAN_POINT('Ctrl Pts',(2.05971511413777,3.71553937395602,-1.87243163954858));
#23605=CARTESIAN_POINT('Ctrl Pts',(2.17843332409981,3.594539256238,2.09535691937294));
#23606=CARTESIAN_POINT('Ctrl Pts',(2.29715153406184,0.201519007352503,4.15579392822546));
#23607=CARTESIAN_POINT('Ctrl Pts',(2.40115216004538,-2.93156287124292,2.64685160308012));
#23608=CARTESIAN_POINT('Ctrl Pts',(2.4655800493749,-3.51529457426641,0.733536282306892));
#23609=CARTESIAN_POINT('Ctrl Pts',(2.49043520205041,-3.51954048850984,-0.00220771176014333));
#23610=CARTESIAN_POINT('Origin',(-7.03243520205041,0.,0.));
#23611=CARTESIAN_POINT('',(0.842564797949603,-3.52020153404575,-0.00255030679734297));
#23612=CARTESIAN_POINT('',(0.990435202050402,-3.5294422032389,-0.000147415198692435));
#23613=CARTESIAN_POINT('',(-7.03243520205041,-3.52375,3.2169090177286E-13));
#23614=CARTESIAN_POINT('Ctrl Pts',(0.842564797949603,-3.52020153404575,
-0.00255030679734352));
#23615=CARTESIAN_POINT('Ctrl Pts',(0.856210381270448,-3.52292703156673,
-0.406286099867594));
#23616=CARTESIAN_POINT('Ctrl Pts',(0.909428701245306,-3.2726899909767,-1.97759684475512));
#23617=CARTESIAN_POINT('Ctrl Pts',(1.00221975787418,-0.961799304980866,
-4.04798401530169));
#23618=CARTESIAN_POINT('Ctrl Pts',(1.12093796783622,2.87028951964572,-3.01208740985575));
#23619=CARTESIAN_POINT('Ctrl Pts',(1.23965617779825,4.0896248253724,0.765637824886821));
#23620=CARTESIAN_POINT('Ctrl Pts',(1.35837438776029,1.586275858193,3.84642189481521));
#23621=CARTESIAN_POINT('Ctrl Pts',(1.47601059447741,-2.32504492362501,3.42973592687219));
#23622=CARTESIAN_POINT('Ctrl Pts',(1.55407406454052,-3.5267219567949,1.13066884340344));
#23623=CARTESIAN_POINT('Ctrl Pts',(1.59256479794961,-3.5293292687682,-0.000582581467793819));
#23624=CARTESIAN_POINT('Ctrl Pts',(0.990435202050402,-3.5294422032389,-0.000147415198692102));
#23625=CARTESIAN_POINT('Ctrl Pts',(0.99070720952674,-3.52944710988525,-0.00814108865577569));
#23626=CARTESIAN_POINT('Ctrl Pts',(1.03055195365709,-3.52581082233263,-1.17908178703684));
#23627=CARTESIAN_POINT('Ctrl Pts',(1.10996943444146,-2.24309286528101,-3.50424991716136));
#23628=CARTESIAN_POINT('Ctrl Pts',(1.22868764440349,1.71622596930723,-3.79022446650269));
#23629=CARTESIAN_POINT('Ctrl Pts',(1.34740585436554,4.11330677534691,-0.626051480379392));
#23630=CARTESIAN_POINT('Ctrl Pts',(1.46612406432757,2.7661462154741,3.10800067548548));
#23631=CARTESIAN_POINT('Ctrl Pts',(1.58484227428961,-1.09896879073751,4.01291672990917));
#23632=CARTESIAN_POINT('Ctrl Pts',(1.67627932019722,-3.30540671418036,1.89644473864501));
#23633=CARTESIAN_POINT('Ctrl Pts',(1.72814362945082,-3.52400110003897,0.366307433305029));
#23634=CARTESIAN_POINT('Ctrl Pts',(1.74043520205041,-3.52117028029313,0.00288554803045071));
#23635=CARTESIAN_POINT('Origin',(-7.03243520205041,0.,0.));
#23636=CARTESIAN_POINT('',(0.0925647979496037,-3.520391836502,0.00262959689127293));
#23637=CARTESIAN_POINT('',(0.240435202050404,-3.52076490314647,-0.00276491524723754));
#23638=CARTESIAN_POINT('',(-7.03243520205041,-3.52375,3.2169090177286E-13));
#23639=CARTESIAN_POINT('Ctrl Pts',(0.0925647979496036,-3.520391836502,0.0026295968912728));
#23640=CARTESIAN_POINT('Ctrl Pts',(0.11877396134637,-3.51497474974621,-0.772722847635471));
#23641=CARTESIAN_POINT('Ctrl Pts',(0.18455586139715,-2.88124574942044,-2.72681485469593));
#23642=CARTESIAN_POINT('Ctrl Pts',(0.289910498101944,0.342796707198351,
-4.1465314310558));
#23643=CARTESIAN_POINT('Ctrl Pts',(0.408628708063982,3.66374931913409,-1.97184518097748));
#23644=CARTESIAN_POINT('Ctrl Pts',(0.52734691802602,3.64968159238416,1.99776294024389));
#23645=CARTESIAN_POINT('Ctrl Pts',(0.64606512798806,0.313399030476065,4.14885689544678));
#23646=CARTESIAN_POINT('Ctrl Pts',(0.751137754629253,-2.89189715861612,
2.71018649449324));
#23647=CARTESIAN_POINT('Ctrl Pts',(0.816637644616435,-3.51502297989571,
0.764563825804819));
#23648=CARTESIAN_POINT('Ctrl Pts',(0.842564797949603,-3.52020153404575,
-0.00255030679734352));
#23649=CARTESIAN_POINT('Ctrl Pts',(0.240435202050404,-3.52076490314647,
-0.00276491524723779));
#23650=CARTESIAN_POINT('Ctrl Pts',(0.253270789602664,-3.52357456820614,
-0.382381961104795));
#23651=CARTESIAN_POINT('Ctrl Pts',(0.305679113808936,-3.29246765048336,
-1.92904800422628));
#23652=CARTESIAN_POINT('Ctrl Pts',(0.397660174669222,-1.04400082814246,
-4.02756692744365));
#23653=CARTESIAN_POINT('Ctrl Pts',(0.516378384631262,2.80838075407454,-3.06989097922772));
#23654=CARTESIAN_POINT('Ctrl Pts',(0.635096594593299,4.10436283463961,0.682230757023696));
#23655=CARTESIAN_POINT('Ctrl Pts',(0.75381480455534,1.66424499718303,3.81333471826842));
#23656=CARTESIAN_POINT('Ctrl Pts',(0.87226100704104,-2.28173208074985,3.47403364657438));
#23657=CARTESIAN_POINT('Ctrl Pts',(0.951134472872727,-3.5287332713303,1.15481052897661));
#23658=CARTESIAN_POINT('Ctrl Pts',(0.990435202050402,-3.5294422032389,-0.000147415198692102));
#23659=CARTESIAN_POINT('Origin',(-7.03243520205041,0.,0.));
#23660=CARTESIAN_POINT('',(-0.657435202050397,-3.5293831919679,0.000432089568584395));
#23661=CARTESIAN_POINT('',(-0.509564797949596,-3.51986320972577,0.00238942109789531));
#23662=CARTESIAN_POINT('',(-7.03243520205041,-3.52375,3.2169090177286E-13));
#23663=CARTESIAN_POINT('Ctrl Pts',(-0.657435202050397,-3.5293831919679,
0.00043208956858453));
#23664=CARTESIAN_POINT('Ctrl Pts',(-0.618662458577708,-3.52740142174523,
-1.13906086225041));
#23665=CARTESIAN_POINT('Ctrl Pts',(-0.540316978451006,-2.31006131649313,
-3.4451963897398));
#23666=CARTESIAN_POINT('Ctrl Pts',(-0.422398761670289,1.61349801702105,
-3.83508235117171));
#23667=CARTESIAN_POINT('Ctrl Pts',(-0.303680551708251,4.09494865907512,
-0.736632860208229));
#23668=CARTESIAN_POINT('Ctrl Pts',(-0.184962341746212,2.84886887415203,
3.0323552940062));
#23669=CARTESIAN_POINT('Ctrl Pts',(-0.0662441317841732,-0.990465746173143,
4.04106546554956));
#23670=CARTESIAN_POINT('Ctrl Pts',(0.0262649147810988,-3.2796457848887,
1.9606934969984));
#23671=CARTESIAN_POINT('Ctrl Pts',(0.0792012246923576,-3.52315391000301,
0.397967633278049));
#23672=CARTESIAN_POINT('Ctrl Pts',(0.0925647979496036,-3.520391836502,0.0026295968912728));
#23673=CARTESIAN_POINT('Ctrl Pts',(-0.509564797949596,-3.51986320972577,
0.00238942109789472));
#23674=CARTESIAN_POINT('Ctrl Pts',(-0.484165630321414,-3.51513982509849,
-0.749284878623226));
#23675=CARTESIAN_POINT('Ctrl Pts',(-0.419193726039219,-2.91159584547546,
-2.67901671514931));
#23676=CARTESIAN_POINT('Ctrl Pts',(-0.31464908510301,0.258318855548078,
-4.15265029265267));
#23677=CARTESIAN_POINT('Ctrl Pts',(-0.195930875140972,3.62285133778538,
-2.04601595020828));
#23678=CARTESIAN_POINT('Ctrl Pts',(-0.0772126651789335,3.68959190165954,
1.92305607911166));
#23679=CARTESIAN_POINT('Ctrl Pts',(0.0415055447831062,0.397788263499511,
4.14161774933685));
#23680=CARTESIAN_POINT('Ctrl Pts',(0.147388167192885,-2.86105940473166,
2.75790715554717));
#23681=CARTESIAN_POINT('Ctrl Pts',(0.213698052948651,-3.51491223506092,
0.787995734807595));
#23682=CARTESIAN_POINT('Ctrl Pts',(0.240435202050404,-3.52076490314647,
-0.00276491524723779));
#23683=CARTESIAN_POINT('Origin',(-7.03243520205041,0.,0.));
#23684=CARTESIAN_POINT('',(-1.4074352020504,-3.52158194415915,-0.00298345148167371));
#23685=CARTESIAN_POINT('',(-1.2595647979496,-3.52918899675462,0.000859749148777282));
#23686=CARTESIAN_POINT('',(-7.03243520205041,-3.52375,3.2169090177286E-13));
#23687=CARTESIAN_POINT('Ctrl Pts',(-1.4074352020504,-3.52158194415915,-0.00298345148167414));
#23688=CARTESIAN_POINT('Ctrl Pts',(-1.3956716151558,-3.5244070910839,-0.350691598451789));
#23689=CARTESIAN_POINT('Ctrl Pts',(-1.34433529160719,-3.31770284706483,
-1.86480632578787));
#23690=CARTESIAN_POINT('Ctrl Pts',(-1.25342623140456,-1.15212076721019,
-3.99798076895909));
#23691=CARTESIAN_POINT('Ctrl Pts',(-1.13470802144252,2.72466151947467,-3.14443191936036));
#23692=CARTESIAN_POINT('Ctrl Pts',(-1.01598981148048,4.12125185197025,0.571415491416797));
#23693=CARTESIAN_POINT('Ctrl Pts',(-0.897271601518446,1.76636861191941,
3.76711752113286));
#23694=CARTESIAN_POINT('Ctrl Pts',(-0.778553391556407,-2.19639626337378,
3.53370569592844));
#23695=CARTESIAN_POINT('Ctrl Pts',(-0.698607925067057,-3.51858688310483,
1.21041940197939));
#23696=CARTESIAN_POINT('Ctrl Pts',(-0.65823519523172,-3.52942408158579,
0.0239431055549515));
#23697=CARTESIAN_POINT('Ctrl Pts',(-0.657435202050397,-3.5293831919679,
0.00043208956858453));
#23698=CARTESIAN_POINT('Ctrl Pts',(-1.2595647979496,-3.52918899675462,0.000859749148777187));
#23699=CARTESIAN_POINT('Ctrl Pts',(-1.22160205024549,-3.5255086737848,-1.11499301985354));
#23700=CARTESIAN_POINT('Ctrl Pts',(-1.14406656588737,-2.3528218011688,-3.40068520645428));
#23701=CARTESIAN_POINT('Ctrl Pts',(-1.02695834487524,1.53509675153174,-3.86713214768211));
#23702=CARTESIAN_POINT('Ctrl Pts',(-0.908240134913205,4.07910533073667,
-0.819837047806264));
#23703=CARTESIAN_POINT('Ctrl Pts',(-0.789521924951166,2.91000527267733,
2.97373542824345));
#23704=CARTESIAN_POINT('Ctrl Pts',(-0.670803714989128,-0.908000571423945,
4.06039013476461));
#23705=CARTESIAN_POINT('Ctrl Pts',(-0.57748467265527,-3.25946475739031,
2.00924411164542));
#23706=CARTESIAN_POINT('Ctrl Pts',(-0.523738366975427,-3.52249901334856,
0.421848346996679));
#23707=CARTESIAN_POINT('Ctrl Pts',(-0.509564797949596,-3.51986320972577,
0.00238942109789472));
#23708=CARTESIAN_POINT('Origin',(-7.03243520205041,0.,0.));
#23709=CARTESIAN_POINT('',(-2.1574352020504,-3.51925399927358,0.00201712429989166));
#23710=CARTESIAN_POINT('',(-2.0095647979496,-3.52224349536472,-0.00309508648049711));
#23711=CARTESIAN_POINT('',(-7.03243520205041,-3.52375,3.2169090177286E-13));
#23712=CARTESIAN_POINT('Ctrl Pts',(-2.1574352020504,-3.51925399927358,0.0020171242998911));
#23713=CARTESIAN_POINT('Ctrl Pts',(-2.13310803507988,-3.51547616379199,
-0.718244932452376));
#23714=CARTESIAN_POINT('Ctrl Pts',(-2.06920813145534,-2.95062385292651,
-2.61558954155717));
#23715=CARTESIAN_POINT('Ctrl Pts',(-1.96573549117679,0.14635662574293,-4.15810199844688));
#23716=CARTESIAN_POINT('Ctrl Pts',(-1.84701728121476,3.56641872576227,-2.14286956292151));
#23717=CARTESIAN_POINT('Ctrl Pts',(-1.72829907125272,3.74005811760244,1.82296400626149));
#23718=CARTESIAN_POINT('Ctrl Pts',(-1.60958086129068,0.509215159922919,
4.12939855331646));
#23719=CARTESIAN_POINT('Ctrl Pts',(-1.50262623822324,-2.81908498068768,
2.82086507657426));
#23720=CARTESIAN_POINT('Ctrl Pts',(-1.43524435180981,-3.51490328954244,
0.818999504762706));
#23721=CARTESIAN_POINT('Ctrl Pts',(-1.4074352020504,-3.52158194415915,-0.00298345148167414));
#23722=CARTESIAN_POINT('Ctrl Pts',(-2.0095647979496,-3.52224349536472,-0.00309508648049749));
#23723=CARTESIAN_POINT('Ctrl Pts',(-1.99861120682358,-3.52501216975828,
-0.326707139459239));
#23724=CARTESIAN_POINT('Ctrl Pts',(-1.94808487904356,-3.33607112434554,
-1.81628010136597));
#23725=CARTESIAN_POINT('Ctrl Pts',(-1.85798581460952,-1.233264991575,-3.97369985590045));
#23726=CARTESIAN_POINT('Ctrl Pts',(-1.73926760464748,2.66008892032246,-3.19924366376966));
#23727=CARTESIAN_POINT('Ctrl Pts',(-1.62054939468544,4.13202971706382,0.487404864048419));
#23728=CARTESIAN_POINT('Ctrl Pts',(-1.5018311847234,1.8426861173841,3.73038080589689));
#23729=CARTESIAN_POINT('Ctrl Pts',(-1.38311297476136,-2.12400905413959,
3.57768341558217));
#23730=CARTESIAN_POINT('Ctrl Pts',(-1.30235751250343,-3.50709119758703,
1.25853137590997));
#23731=CARTESIAN_POINT('Ctrl Pts',(-1.26117478689951,-3.52934507816789,
0.0481827364578268));
#23732=CARTESIAN_POINT('Ctrl Pts',(-1.2595647979496,-3.52918899675462,0.000859749148777187));
#23733=CARTESIAN_POINT('Origin',(-7.03243520205041,0.,0.));
#23734=CARTESIAN_POINT('',(-2.9074352020504,-3.52876079344158,0.00139557051607088));
#23735=CARTESIAN_POINT('',(-2.7595647979496,-3.5188691614322,0.0017004510770105));
#23736=CARTESIAN_POINT('',(-7.03243520205041,-3.52375,3.2169090177286E-13));
#23737=CARTESIAN_POINT('Ctrl Pts',(-2.9074352020504,-3.52876079344158,0.0013955705160707));
#23738=CARTESIAN_POINT('Ctrl Pts',(-2.87054445500395,-3.52327543776816,
-1.08329821888431));
#23739=CARTESIAN_POINT('Ctrl Pts',(-2.7940809713035,-2.40811731696173,-3.34129519327353));
#23740=CARTESIAN_POINT('Ctrl Pts',(-2.67804475094903,1.43036271770746,-3.90708267059147));
#23741=CARTESIAN_POINT('Ctrl Pts',(-2.55932654098699,4.05553922750062,-0.929426740059659));
#23742=CARTESIAN_POINT('Ctrl Pts',(-2.44060833102495,2.9890587402779,2.89426334951592));
#23743=CARTESIAN_POINT('Ctrl Pts',(-2.32189012106291,-0.798287948035305,
4.08337713718073));
#23744=CARTESIAN_POINT('Ctrl Pts',(-2.22749907807139,-3.23179197730365,
2.07349551989286));
#23745=CARTESIAN_POINT('Ctrl Pts',(-2.17268077173389,-3.5216215274842,0.453397483956963));
#23746=CARTESIAN_POINT('Ctrl Pts',(-2.1574352020504,-3.51925399927358,0.0020171242998911));
#23747=CARTESIAN_POINT('Ctrl Pts',(-2.7595647979496,-3.5188691614322,0.00170045107701029));
#23748=CARTESIAN_POINT('Ctrl Pts',(-2.73604762674766,-3.51581077998374,
-0.694770743658778));
#23749=CARTESIAN_POINT('Ctrl Pts',(-2.67295771889171,-2.97926278234442,
-2.56755066425432));
#23750=CARTESIAN_POINT('Ctrl Pts',(-2.57029507438175,0.0616839434797912,
-4.16021972695477));
#23751=CARTESIAN_POINT('Ctrl Pts',(-2.45157686441971,3.52205953641558,-2.21502363553932));
#23752=CARTESIAN_POINT('Ctrl Pts',(-2.33285865445767,3.77639149338881,1.74645365601417));
#23753=CARTESIAN_POINT('Ctrl Pts',(-2.21414044449563,0.593167728051762,
4.11817740399618));
#23754=CARTESIAN_POINT('Ctrl Pts',(-2.10637582565961,-2.78648195150766,
2.86827122209582));
#23755=CARTESIAN_POINT('Ctrl Pts',(-2.0381839434776,-3.5150096033491,0.842426745790324));
#23756=CARTESIAN_POINT('Ctrl Pts',(-2.0095647979496,-3.52224349536472,-0.00309508648049749));
#23757=CARTESIAN_POINT('Origin',(-7.03243520205041,0.,0.));
#23758=CARTESIAN_POINT('',(-3.6574352020504,-3.52316113046627,-0.0031674687847638));
#23759=CARTESIAN_POINT('',(-3.5095647979496,-3.52832659366549,0.00176786622774379));
#23760=CARTESIAN_POINT('',(-7.03243520205041,-3.52375,3.2169090177286E-13));
#23761=CARTESIAN_POINT('Ctrl Pts',(-3.6574352020504,-3.52316113046627,-0.00316746878476385));
#23762=CARTESIAN_POINT('Ctrl Pts',(-3.64755361158204,-3.52577324579835,
-0.294914834651217));
#23763=CARTESIAN_POINT('Ctrl Pts',(-3.59809928445968,-3.35947056833859,
-1.7520841168655));
#23764=CARTESIAN_POINT('Ctrl Pts',(-3.5090722206833,-1.33986509473402,-3.93903455379817));
#23765=CARTESIAN_POINT('Ctrl Pts',(-3.39035401072126,2.57293885887897,-3.26974286547831));
#23766=CARTESIAN_POINT('Ctrl Pts',(-3.27163580075922,4.14366027205377,0.375915015385937));
#23767=CARTESIAN_POINT('Ctrl Pts',(-3.15291759079718,1.94251026639215,3.67938666679367));
#23768=CARTESIAN_POINT('Ctrl Pts',(-3.03419938083515,-2.0268587551866,3.63360373818345));
#23769=CARTESIAN_POINT('Ctrl Pts',(-2.95237191791955,-3.49109730462382,
1.3222721650432));
#23770=CARTESIAN_POINT('Ctrl Pts',(-2.91011719165797,-3.52915958360139,
0.0802537586385255));
#23771=CARTESIAN_POINT('Ctrl Pts',(-2.9074352020504,-3.52876079344158,0.0013955705160707));
#23772=CARTESIAN_POINT('Ctrl Pts',(-3.5095647979496,-3.52832659366549,0.00176786622774375));
#23773=CARTESIAN_POINT('Ctrl Pts',(-3.47348404667174,-3.52178655096766,
-1.05945570162635));
#23774=CARTESIAN_POINT('Ctrl Pts',(-3.39783055873987,-2.44892508739056,
-3.29607736830673));
#23775=CARTESIAN_POINT('Ctrl Pts',(-3.28260433415398,1.35053375419133,-3.93538965177946));
#23776=CARTESIAN_POINT('Ctrl Pts',(-3.16388612419195,4.03577955172485,-1.0117887612591));
#23777=CARTESIAN_POINT('Ctrl Pts',(-3.0451679142299,3.04735509174485,2.83281838700313));
#23778=CARTESIAN_POINT('Ctrl Pts',(-2.92644970426787,-0.715001293115481,
4.09878106793642));
#23779=CARTESIAN_POINT('Ctrl Pts',(-2.83124866550776,-3.21014363212566,
2.122033607616));
#23780=CARTESIAN_POINT('Ctrl Pts',(-2.77562036340167,-3.52095716951368,
0.477192964889438));
#23781=CARTESIAN_POINT('Ctrl Pts',(-2.7595647979496,-3.5188691614322,0.00170045107701029));
#23782=CARTESIAN_POINT('Origin',(-7.03243520205041,0.,0.));
#23783=CARTESIAN_POINT('',(-4.4074352020504,-3.51846707334834,0.00124753304639253));
#23784=CARTESIAN_POINT('',(-4.2595647979496,-3.52387435346743,-0.00316304557197139));
#23785=CARTESIAN_POINT('',(-7.03243520205041,-3.52375,3.2169090177286E-13));
#23786=CARTESIAN_POINT('Ctrl Pts',(-4.4074352020504,-3.51846707334834,0.00124753304639239));
#23787=CARTESIAN_POINT('Ctrl Pts',(-4.38499003150612,-3.51634687456568,
-0.663667541133016));
#23788=CARTESIAN_POINT('Ctrl Pts',(-4.32297212430784,-3.01605608718915,
-2.50384701489226));
#23789=CARTESIAN_POINT('Ctrl Pts',(-4.22138148045554,-0.0504100535793502,
-4.16036696958348));
#23790=CARTESIAN_POINT('Ctrl Pts',(-4.10266327049349,3.46111018837926,-2.30910306912985));
#23791=CARTESIAN_POINT('Ctrl Pts',(-3.98394506053146,3.82206891947539,1.64408864020745));
#23792=CARTESIAN_POINT('Ctrl Pts',(-3.86522685056942,0.703892139470341,
4.1007027146119));
#23793=CARTESIAN_POINT('Ctrl Pts',(-3.75639023107573,-2.7421442575855,2.93077227568166));
#23794=CARTESIAN_POINT('Ctrl Pts',(-3.68712634823606,-3.51531252568681,
0.87344381327186));
#23795=CARTESIAN_POINT('Ctrl Pts',(-3.6574352020504,-3.52316113046627,-0.00316746878476385));
#23796=CARTESIAN_POINT('Ctrl Pts',(-4.2595647979496,-3.52387435346743,-0.0031630455719716));
#23797=CARTESIAN_POINT('Ctrl Pts',(-4.25049320324983,-3.52631361922211,
-0.270857380598162));
#23798=CARTESIAN_POINT('Ctrl Pts',(-4.20184887189605,-3.37647405540411,
-1.70360378513277));
#23799=CARTESIAN_POINT('Ctrl Pts',(-4.11363180388825,-1.41977030063975,
-3.9109435932429));
#23800=CARTESIAN_POINT('Ctrl Pts',(-3.99491359392623,2.50584675349696,-3.32144046072034));
#23801=CARTESIAN_POINT('Ctrl Pts',(-3.87619538396417,4.1504539432636,0.29148889536334));
#23802=CARTESIAN_POINT('Ctrl Pts',(-3.75747717400214,2.01700539684609,3.63908250952178));
#23803=CARTESIAN_POINT('Ctrl Pts',(-3.6387589640401,-1.9524731306016,3.67410969416408));
#23804=CARTESIAN_POINT('Ctrl Pts',(-3.55612150535592,-3.47841478275052,
1.37048332710352));
#23805=CARTESIAN_POINT('Ctrl Pts',(-3.51305678332575,-3.52895955535979,
0.104475738113171));
#23806=CARTESIAN_POINT('Ctrl Pts',(-3.5095647979496,-3.52832659366549,0.00176786622774375));
#23807=CARTESIAN_POINT('Origin',(-7.03243520205041,0.,0.));
#23808=CARTESIAN_POINT('',(-5.1574352020504,-3.52758964538326,0.00244996322663533));
#23809=CARTESIAN_POINT('',(-5.0095647979496,-3.51824182757685,0.00090084872823859));
#23810=CARTESIAN_POINT('',(-7.03243520205041,-3.52375,3.2169090177286E-13));
#23811=CARTESIAN_POINT('Ctrl Pts',(-5.1574352020504,-3.52758964538326,0.0024499632266353));
#23812=CARTESIAN_POINT('Ctrl Pts',(-5.1224264514302,-3.52001727243588,-1.02772586371769));
#23813=CARTESIAN_POINT('Ctrl Pts',(-5.04784496415598,-2.50172051158108,
-3.23619325292719));
#23814=CARTESIAN_POINT('Ctrl Pts',(-4.93369074022778,1.24406479104381,-3.9701278679622));
#23815=CARTESIAN_POINT('Ctrl Pts',(-4.81497253026572,4.0070387833704,-1.12025498671569));
#23816=CARTESIAN_POINT('Ctrl Pts',(-4.69625432030369,3.12257273473017,2.74975698427391));
#23817=CARTESIAN_POINT('Ctrl Pts',(-4.57753611034165,-0.604329863247786,
4.116523575551));
#23818=CARTESIAN_POINT('Ctrl Pts',(-4.48126307092388,-3.18049740052607,
2.18625513612602));
#23819=CARTESIAN_POINT('Ctrl Pts',(-4.42456276816014,-3.52008496458887,
0.508634049353034));
#23820=CARTESIAN_POINT('Ctrl Pts',(-4.4074352020504,-3.51846707334834,0.00124753304639239));
#23821=CARTESIAN_POINT('Ctrl Pts',(-5.0095647979496,-3.51824182757685,0.000900848728238278));
#23822=CARTESIAN_POINT('Ctrl Pts',(-4.98792962317391,-3.51681057818972,
-0.640128378860598));
#23823=CARTESIAN_POINT('Ctrl Pts',(-4.92672171174421,-3.04304236494483,
-2.45565670627494));
#23824=CARTESIAN_POINT('Ctrl Pts',(-4.82594106366048,-0.135078114281208,
-4.15845351012906));
#23825=CARTESIAN_POINT('Ctrl Pts',(-4.70722285369845,3.41338373023632,-2.37909235958642));
#23826=CARTESIAN_POINT('Ctrl Pts',(-4.58850464373641,3.85474686870501,1.56595294230416));
#23827=CARTESIAN_POINT('Ctrl Pts',(-4.46978643377438,0.787218792347394,
4.08552098175258));
#23828=CARTESIAN_POINT('Ctrl Pts',(-4.3601398185121,-2.70773509524305,2.97780255324554));
#23829=CARTESIAN_POINT('Ctrl Pts',(-4.29006593990384,-3.5156728857531,0.896897327847196));
#23830=CARTESIAN_POINT('Ctrl Pts',(-4.2595647979496,-3.52387435346743,-0.0031630455719716));
#23831=CARTESIAN_POINT('Origin',(15.2,0.,0.));
#23832=CARTESIAN_POINT('',(15.4,4.99875513987758,0.111566354908184));
#23833=CARTESIAN_POINT('',(15.4,5.,6.12323399573677E-16));
#23834=CARTESIAN_POINT('Origin',(15.4,0.,0.));
#23835=CARTESIAN_POINT('',(15.,4.6,5.63337527607783E-16));
#23836=CARTESIAN_POINT('',(15.2,4.8,5.87830463590729E-16));
#23837=CARTESIAN_POINT('Origin',(15.,0.,0.));
#23838=CARTESIAN_POINT('',(15.4,4.99875513987758,-0.111566354908184));
#23839=CARTESIAN_POINT('Origin',(15.4,0.,0.));
#23840=CARTESIAN_POINT('',(15.4,4.85730218634588,-1.18600820845369));
#23841=CARTESIAN_POINT('Origin',(15.4,0.,0.));
#23842=CARTESIAN_POINT('',(15.4,4.79955119146007,-1.40153785555518));
#23843=CARTESIAN_POINT('Origin',(15.4,0.,0.));
#23844=CARTESIAN_POINT('',(15.4,4.38483211588611,-2.40275827238067));
#23845=CARTESIAN_POINT('Origin',(15.4,0.,0.));
#23846=CARTESIAN_POINT('',(15.4,4.27326576097792,-2.59599686749691));
#23847=CARTESIAN_POINT('Origin',(15.4,0.,0.));
#23848=CARTESIAN_POINT('',(15.4,3.61354298300638,-3.4557643307907));
#23849=CARTESIAN_POINT('Origin',(15.4,0.,0.));
#23850=CARTESIAN_POINT('',(15.4,3.4557643307907,-3.61354298300639));
#23851=CARTESIAN_POINT('Origin',(15.4,0.,0.));
#23852=CARTESIAN_POINT('',(15.4,2.5959968674969,-4.27326576097793));
#23853=CARTESIAN_POINT('Origin',(15.4,0.,0.));
#23854=CARTESIAN_POINT('',(15.4,2.40275827238067,-4.38483211588611));
#23855=CARTESIAN_POINT('Origin',(15.4,0.,0.));
#23856=CARTESIAN_POINT('',(15.4,1.40153785555518,-4.79955119146007));
#23857=CARTESIAN_POINT('Origin',(15.4,0.,0.));
#23858=CARTESIAN_POINT('',(15.4,1.18600820845368,-4.85730218634588));
#23859=CARTESIAN_POINT('Origin',(15.4,0.,0.));
#23860=CARTESIAN_POINT('',(15.4,0.111566354908183,-4.99875513987758));
#23861=CARTESIAN_POINT('Origin',(15.4,0.,0.));
#23862=CARTESIAN_POINT('',(15.4,-0.111566354908184,-4.99875513987758));
#23863=CARTESIAN_POINT('Origin',(15.4,0.,0.));
#23864=CARTESIAN_POINT('',(15.4,-1.18600820845369,-4.85730218634588));
#23865=CARTESIAN_POINT('Origin',(15.4,0.,0.));
#23866=CARTESIAN_POINT('',(15.4,-1.40153785555518,-4.79955119146007));
#23867=CARTESIAN_POINT('Origin',(15.4,0.,0.));
#23868=CARTESIAN_POINT('',(15.4,-2.40275827238067,-4.38483211588611));
#23869=CARTESIAN_POINT('Origin',(15.4,0.,0.));
#23870=CARTESIAN_POINT('',(15.4,-2.59599686749691,-4.27326576097792));
#23871=CARTESIAN_POINT('Origin',(15.4,0.,0.));
#23872=CARTESIAN_POINT('',(15.4,-3.4557643307907,-3.61354298300638));
#23873=CARTESIAN_POINT('Origin',(15.4,0.,0.));
#23874=CARTESIAN_POINT('',(15.4,-3.61354298300639,-3.4557643307907));
#23875=CARTESIAN_POINT('Origin',(15.4,0.,0.));
#23876=CARTESIAN_POINT('',(15.4,-4.27326576097793,-2.5959968674969));
#23877=CARTESIAN_POINT('Origin',(15.4,0.,0.));
#23878=CARTESIAN_POINT('',(15.4,-4.38483211588611,-2.40275827238067));
#23879=CARTESIAN_POINT('Origin',(15.4,0.,0.));
#23880=CARTESIAN_POINT('',(15.4,-4.79955119146007,-1.40153785555518));
#23881=CARTESIAN_POINT('Origin',(15.4,0.,0.));
#23882=CARTESIAN_POINT('',(15.4,-4.85730218634588,-1.18600820845368));
#23883=CARTESIAN_POINT('Origin',(15.4,0.,0.));
#23884=CARTESIAN_POINT('',(15.4,-4.99875513987758,-0.111566354908183));
#23885=CARTESIAN_POINT('Origin',(15.4,0.,0.));
#23886=CARTESIAN_POINT('',(15.4,-4.99875513987758,0.111566354908184));
#23887=CARTESIAN_POINT('Origin',(15.4,0.,0.));
#23888=CARTESIAN_POINT('',(15.4,-4.85730218634588,1.18600820845369));
#23889=CARTESIAN_POINT('Origin',(15.4,0.,0.));
#23890=CARTESIAN_POINT('',(15.4,-4.79955119146007,1.40153785555518));
#23891=CARTESIAN_POINT('Origin',(15.4,0.,0.));
#23892=CARTESIAN_POINT('',(15.4,-4.38483211588611,2.40275827238067));
#23893=CARTESIAN_POINT('Origin',(15.4,0.,0.));
#23894=CARTESIAN_POINT('',(15.4,-4.27326576097792,2.59599686749691));
#23895=CARTESIAN_POINT('Origin',(15.4,0.,0.));
#23896=CARTESIAN_POINT('',(15.4,-3.61354298300639,3.4557643307907));
#23897=CARTESIAN_POINT('Origin',(15.4,0.,0.));
#23898=CARTESIAN_POINT('',(15.4,-3.4557643307907,3.61354298300639));
#23899=CARTESIAN_POINT('Origin',(15.4,0.,0.));
#23900=CARTESIAN_POINT('',(15.4,-2.5959968674969,4.27326576097793));
#23901=CARTESIAN_POINT('Origin',(15.4,0.,0.));
#23902=CARTESIAN_POINT('',(15.4,-2.40275827238067,4.38483211588611));
#23903=CARTESIAN_POINT('Origin',(15.4,0.,0.));
#23904=CARTESIAN_POINT('',(15.4,-1.40153785555518,4.79955119146007));
#23905=CARTESIAN_POINT('Origin',(15.4,0.,0.));
#23906=CARTESIAN_POINT('',(15.4,-1.18600820845369,4.85730218634588));
#23907=CARTESIAN_POINT('Origin',(15.4,0.,0.));
#23908=CARTESIAN_POINT('',(15.4,-0.111566354908183,4.99875513987758));
#23909=CARTESIAN_POINT('Origin',(15.4,0.,0.));
#23910=CARTESIAN_POINT('',(15.4,0.111566354908184,4.99875513987758));
#23911=CARTESIAN_POINT('Origin',(15.4,0.,0.));
#23912=CARTESIAN_POINT('',(15.4,1.18600820845369,4.85730218634588));
#23913=CARTESIAN_POINT('Origin',(15.4,0.,0.));
#23914=CARTESIAN_POINT('',(15.4,1.40153785555518,4.79955119146007));
#23915=CARTESIAN_POINT('Origin',(15.4,0.,0.));
#23916=CARTESIAN_POINT('',(15.4,2.40275827238067,4.38483211588611));
#23917=CARTESIAN_POINT('Origin',(15.4,0.,0.));
#23918=CARTESIAN_POINT('',(15.4,2.59599686749691,4.27326576097793));
#23919=CARTESIAN_POINT('Origin',(15.4,0.,0.));
#23920=CARTESIAN_POINT('',(15.4,3.4557643307907,3.61354298300638));
#23921=CARTESIAN_POINT('Origin',(15.4,0.,0.));
#23922=CARTESIAN_POINT('',(15.4,3.61354298300639,3.4557643307907));
#23923=CARTESIAN_POINT('Origin',(15.4,0.,0.));
#23924=CARTESIAN_POINT('',(15.4,4.27326576097793,2.59599686749691));
#23925=CARTESIAN_POINT('Origin',(15.4,0.,0.));
#23926=CARTESIAN_POINT('',(15.4,4.38483211588611,2.40275827238067));
#23927=CARTESIAN_POINT('Origin',(15.4,0.,0.));
#23928=CARTESIAN_POINT('',(15.4,4.79955119146007,1.40153785555518));
#23929=CARTESIAN_POINT('Origin',(15.4,0.,0.));
#23930=CARTESIAN_POINT('',(15.4,4.85730218634588,1.18600820845369));
#23931=CARTESIAN_POINT('Origin',(15.4,0.,0.));
#23932=CARTESIAN_POINT('Origin',(15.4,0.,0.));
#23933=CARTESIAN_POINT('Origin',(17.75,0.,0.));
#23934=CARTESIAN_POINT('',(20.5,-5.,-6.12323399573677E-16));
#23935=CARTESIAN_POINT('Origin',(20.5,0.,0.));
#23936=CARTESIAN_POINT('',(20.4,-5.,-6.12323399573677E-16));
#23937=CARTESIAN_POINT('',(17.75,-5.,-6.12323399573677E-16));
#23938=CARTESIAN_POINT('',(20.4,-4.99875513987758,-0.111566354908183));
#23939=CARTESIAN_POINT('Origin',(20.4,0.,0.));
#23940=CARTESIAN_POINT('',(17.75,-4.99875513987758,-0.111566354908183));
#23941=CARTESIAN_POINT('',(20.4,-4.85730218634588,-1.18600820845368));
#23942=CARTESIAN_POINT('',(17.75,-4.85730218634588,-1.18600820845368));
#23943=CARTESIAN_POINT('',(20.4,-4.79955119146007,-1.40153785555518));
#23944=CARTESIAN_POINT('Origin',(20.4,0.,0.));
#23945=CARTESIAN_POINT('',(17.75,-4.79955119146007,-1.40153785555518));
#23946=CARTESIAN_POINT('',(20.4,-4.38483211588611,-2.40275827238067));
#23947=CARTESIAN_POINT('',(17.75,-4.38483211588611,-2.40275827238067));
#23948=CARTESIAN_POINT('',(20.4,-4.27326576097793,-2.5959968674969));
#23949=CARTESIAN_POINT('Origin',(20.4,0.,0.));
#23950=CARTESIAN_POINT('',(17.75,-4.27326576097793,-2.5959968674969));
#23951=CARTESIAN_POINT('',(20.4,-3.61354298300639,-3.4557643307907));
#23952=CARTESIAN_POINT('',(17.75,-3.61354298300639,-3.4557643307907));
#23953=CARTESIAN_POINT('',(20.4,-3.4557643307907,-3.61354298300638));
#23954=CARTESIAN_POINT('Origin',(20.4,0.,0.));
#23955=CARTESIAN_POINT('',(17.75,-3.4557643307907,-3.61354298300638));
#23956=CARTESIAN_POINT('',(20.4,-2.59599686749691,-4.27326576097792));
#23957=CARTESIAN_POINT('',(17.75,-2.59599686749691,-4.27326576097792));
#23958=CARTESIAN_POINT('',(20.4,-2.40275827238067,-4.38483211588611));
#23959=CARTESIAN_POINT('Origin',(20.4,0.,0.));
#23960=CARTESIAN_POINT('',(17.75,-2.40275827238067,-4.38483211588611));
#23961=CARTESIAN_POINT('',(20.4,-1.40153785555518,-4.79955119146007));
#23962=CARTESIAN_POINT('',(17.75,-1.40153785555518,-4.79955119146007));
#23963=CARTESIAN_POINT('',(20.4,-1.18600820845369,-4.85730218634588));
#23964=CARTESIAN_POINT('Origin',(20.4,0.,0.));
#23965=CARTESIAN_POINT('',(17.75,-1.18600820845369,-4.85730218634588));
#23966=CARTESIAN_POINT('',(20.4,-0.111566354908184,-4.99875513987758));
#23967=CARTESIAN_POINT('',(17.75,-0.111566354908184,-4.99875513987758));
#23968=CARTESIAN_POINT('',(20.4,0.111566354908183,-4.99875513987758));
#23969=CARTESIAN_POINT('Origin',(20.4,0.,0.));
#23970=CARTESIAN_POINT('',(17.75,0.111566354908183,-4.99875513987758));
#23971=CARTESIAN_POINT('',(20.4,1.18600820845368,-4.85730218634588));
#23972=CARTESIAN_POINT('',(17.75,1.18600820845368,-4.85730218634588));
#23973=CARTESIAN_POINT('',(20.4,1.40153785555518,-4.79955119146007));
#23974=CARTESIAN_POINT('Origin',(20.4,0.,0.));
#23975=CARTESIAN_POINT('',(17.75,1.40153785555518,-4.79955119146007));
#23976=CARTESIAN_POINT('',(20.4,2.40275827238067,-4.38483211588611));
#23977=CARTESIAN_POINT('',(17.75,2.40275827238067,-4.38483211588611));
#23978=CARTESIAN_POINT('',(20.4,2.5959968674969,-4.27326576097793));
#23979=CARTESIAN_POINT('Origin',(20.4,0.,0.));
#23980=CARTESIAN_POINT('',(17.75,2.5959968674969,-4.27326576097793));
#23981=CARTESIAN_POINT('',(20.4,3.4557643307907,-3.61354298300639));
#23982=CARTESIAN_POINT('',(17.75,3.4557643307907,-3.61354298300639));
#23983=CARTESIAN_POINT('',(20.4,3.61354298300638,-3.4557643307907));
#23984=CARTESIAN_POINT('Origin',(20.4,0.,0.));
#23985=CARTESIAN_POINT('',(17.75,3.61354298300638,-3.4557643307907));
#23986=CARTESIAN_POINT('',(20.4,4.27326576097792,-2.59599686749691));
#23987=CARTESIAN_POINT('',(17.75,4.27326576097792,-2.59599686749691));
#23988=CARTESIAN_POINT('',(20.4,4.38483211588611,-2.40275827238067));
#23989=CARTESIAN_POINT('Origin',(20.4,0.,0.));
#23990=CARTESIAN_POINT('',(17.75,4.38483211588611,-2.40275827238067));
#23991=CARTESIAN_POINT('',(20.4,4.79955119146007,-1.40153785555518));
#23992=CARTESIAN_POINT('',(17.75,4.79955119146007,-1.40153785555518));
#23993=CARTESIAN_POINT('',(20.4,4.85730218634588,-1.18600820845369));
#23994=CARTESIAN_POINT('Origin',(20.4,0.,0.));
#23995=CARTESIAN_POINT('',(17.75,4.85730218634588,-1.18600820845369));
#23996=CARTESIAN_POINT('',(20.4,4.99875513987758,-0.111566354908184));
#23997=CARTESIAN_POINT('',(17.75,4.99875513987758,-0.111566354908184));
#23998=CARTESIAN_POINT('',(20.4,4.99875513987758,0.111566354908184));
#23999=CARTESIAN_POINT('Origin',(20.4,0.,0.));
#24000=CARTESIAN_POINT('',(17.75,4.99875513987758,0.111566354908184));
#24001=CARTESIAN_POINT('',(20.4,4.85730218634588,1.18600820845369));
#24002=CARTESIAN_POINT('',(17.75,4.85730218634588,1.18600820845369));
#24003=CARTESIAN_POINT('',(20.4,4.79955119146007,1.40153785555518));
#24004=CARTESIAN_POINT('Origin',(20.4,0.,0.));
#24005=CARTESIAN_POINT('',(17.75,4.79955119146007,1.40153785555518));
#24006=CARTESIAN_POINT('',(20.4,4.38483211588611,2.40275827238067));
#24007=CARTESIAN_POINT('',(17.75,4.38483211588611,2.40275827238067));
#24008=CARTESIAN_POINT('',(20.4,4.27326576097793,2.59599686749691));
#24009=CARTESIAN_POINT('Origin',(20.4,0.,0.));
#24010=CARTESIAN_POINT('',(17.75,4.27326576097793,2.59599686749691));
#24011=CARTESIAN_POINT('',(20.4,3.61354298300639,3.4557643307907));
#24012=CARTESIAN_POINT('',(17.75,3.61354298300639,3.4557643307907));
#24013=CARTESIAN_POINT('',(20.4,3.4557643307907,3.61354298300638));
#24014=CARTESIAN_POINT('Origin',(20.4,0.,0.));
#24015=CARTESIAN_POINT('',(17.75,3.4557643307907,3.61354298300638));
#24016=CARTESIAN_POINT('',(20.4,2.59599686749691,4.27326576097793));
#24017=CARTESIAN_POINT('',(17.75,2.59599686749691,4.27326576097793));
#24018=CARTESIAN_POINT('',(20.4,2.40275827238067,4.38483211588611));
#24019=CARTESIAN_POINT('Origin',(20.4,0.,0.));
#24020=CARTESIAN_POINT('',(17.75,2.40275827238067,4.38483211588611));
#24021=CARTESIAN_POINT('',(20.4,1.40153785555518,4.79955119146007));
#24022=CARTESIAN_POINT('',(17.75,1.40153785555518,4.79955119146007));
#24023=CARTESIAN_POINT('',(20.4,1.18600820845369,4.85730218634588));
#24024=CARTESIAN_POINT('Origin',(20.4,0.,0.));
#24025=CARTESIAN_POINT('',(17.75,1.18600820845369,4.85730218634588));
#24026=CARTESIAN_POINT('',(20.4,0.111566354908184,4.99875513987758));
#24027=CARTESIAN_POINT('',(17.75,0.111566354908184,4.99875513987758));
#24028=CARTESIAN_POINT('',(20.4,-0.111566354908183,4.99875513987758));
#24029=CARTESIAN_POINT('Origin',(20.4,0.,0.));
#24030=CARTESIAN_POINT('',(17.75,-0.111566354908183,4.99875513987758));
#24031=CARTESIAN_POINT('',(20.4,-1.18600820845369,4.85730218634588));
#24032=CARTESIAN_POINT('',(17.75,-1.18600820845369,4.85730218634588));
#24033=CARTESIAN_POINT('',(20.4,-1.40153785555518,4.79955119146007));
#24034=CARTESIAN_POINT('Origin',(20.4,0.,0.));
#24035=CARTESIAN_POINT('',(17.75,-1.40153785555518,4.79955119146007));
#24036=CARTESIAN_POINT('',(20.4,-2.40275827238067,4.38483211588611));
#24037=CARTESIAN_POINT('',(17.75,-2.40275827238067,4.38483211588611));
#24038=CARTESIAN_POINT('',(20.4,-2.5959968674969,4.27326576097793));
#24039=CARTESIAN_POINT('Origin',(20.4,0.,0.));
#24040=CARTESIAN_POINT('',(17.75,-2.5959968674969,4.27326576097793));
#24041=CARTESIAN_POINT('',(20.4,-3.4557643307907,3.61354298300639));
#24042=CARTESIAN_POINT('',(17.75,-3.4557643307907,3.61354298300639));
#24043=CARTESIAN_POINT('',(20.4,-3.61354298300639,3.4557643307907));
#24044=CARTESIAN_POINT('Origin',(20.4,0.,0.));
#24045=CARTESIAN_POINT('',(17.75,-3.61354298300639,3.4557643307907));
#24046=CARTESIAN_POINT('',(20.4,-4.27326576097792,2.59599686749691));
#24047=CARTESIAN_POINT('',(17.75,-4.27326576097792,2.59599686749691));
#24048=CARTESIAN_POINT('',(20.4,-4.38483211588611,2.40275827238067));
#24049=CARTESIAN_POINT('Origin',(20.4,0.,0.));
#24050=CARTESIAN_POINT('',(17.75,-4.38483211588611,2.40275827238067));
#24051=CARTESIAN_POINT('',(20.4,-4.79955119146007,1.40153785555518));
#24052=CARTESIAN_POINT('',(17.75,-4.79955119146007,1.40153785555518));
#24053=CARTESIAN_POINT('',(20.4,-4.85730218634588,1.18600820845369));
#24054=CARTESIAN_POINT('Origin',(20.4,0.,0.));
#24055=CARTESIAN_POINT('',(17.75,-4.85730218634588,1.18600820845369));
#24056=CARTESIAN_POINT('',(20.4,-4.99875513987758,0.111566354908184));
#24057=CARTESIAN_POINT('',(17.75,-4.99875513987758,0.111566354908184));
#24058=CARTESIAN_POINT('Origin',(20.4,0.,0.));
#24059=CARTESIAN_POINT('Origin',(15.,5.,0.));
#24060=CARTESIAN_POINT('',(15.,-1.03647793659398,-3.81573446232228));
#24061=CARTESIAN_POINT('',(15.,2.28804281094429,-3.22474434572513));
#24062=CARTESIAN_POINT('Origin',(15.,0.,0.));
#24063=CARTESIAN_POINT('Ctrl Pts',(15.,2.29296287427331,-3.22854765929654));
#24064=CARTESIAN_POINT('Ctrl Pts',(15.,2.38802987998202,-3.15422468240186));
#24065=CARTESIAN_POINT('Ctrl Pts',(15.,2.47929003976274,-3.07546894025832));
#24066=CARTESIAN_POINT('Ctrl Pts',(15.,2.56634326510049,-2.99233335005528));
#24067=CARTESIAN_POINT('Ctrl Pts',(15.,2.65493259497213,-2.90773078425721));
#24068=CARTESIAN_POINT('Ctrl Pts',(15.,2.73916570047965,-2.81859185262434));
#24069=CARTESIAN_POINT('Ctrl Pts',(15.,2.81893234754107,-2.72535231130569));
#24070=CARTESIAN_POINT('Ctrl Pts',(15.,2.8655488015903,-2.67086215842129));
#24071=CARTESIAN_POINT('Ctrl Pts',(15.,2.9106390081652,-2.6149708782813));
#24072=CARTESIAN_POINT('Ctrl Pts',(15.,2.95417392507206,-2.55776142184591));
#24073=CARTESIAN_POINT('Ctrl Pts',(15.,2.97044986150209,-2.53637313073853));
#24074=CARTESIAN_POINT('Ctrl Pts',(15.,2.98650835998393,-2.51480057368804));
#24075=CARTESIAN_POINT('Ctrl Pts',(15.,3.00234770735048,-2.49304801108135));
#24076=CARTESIAN_POINT('Ctrl Pts',(15.,3.01345384358298,-2.47779568293138));
#24077=CARTESIAN_POINT('Ctrl Pts',(15.,3.0244501860737,-2.46245759943643));
#24078=CARTESIAN_POINT('Ctrl Pts',(15.,3.03533167348133,-2.44704197570961));
#24079=CARTESIAN_POINT('Ctrl Pts',(15.,3.10579918825424,-2.34721180984998));
#24080=CARTESIAN_POINT('Ctrl Pts',(15.,3.1715131122476,-2.24405067996107));
#24081=CARTESIAN_POINT('Ctrl Pts',(15.,3.23237311287027,-2.13799352531919));
#24082=CARTESIAN_POINT('Ctrl Pts',(15.,3.28913549272338,-2.039077054134));
#24083=CARTESIAN_POINT('Ctrl Pts',(15.,3.34167530236964,-1.93764052209836));
#24084=CARTESIAN_POINT('Ctrl Pts',(15.,3.38987488751025,-1.83402043431015));
#24085=CARTESIAN_POINT('Ctrl Pts',(15.,3.41096220600926,-1.7886866459028));
#24086=CARTESIAN_POINT('Ctrl Pts',(15.,3.43121831216432,-1.74293476505114));
#24087=CARTESIAN_POINT('Ctrl Pts',(15.,3.45063112290763,-1.69679248888462));
#24088=CARTESIAN_POINT('Ctrl Pts',(15.,3.46151559578505,-1.67092120419135));
#24089=CARTESIAN_POINT('Ctrl Pts',(15.,3.47213493890906,-1.64492718836514));
#24090=CARTESIAN_POINT('Ctrl Pts',(15.,3.48248682880138,-1.61881530800709));
#24091=CARTESIAN_POINT('Ctrl Pts',(15.,3.49167793747036,-1.59563141285185));
#24092=CARTESIAN_POINT('Ctrl Pts',(15.,3.50065985969643,-1.57234993370711));
#24093=CARTESIAN_POINT('Ctrl Pts',(15.,3.50942051936889,-1.54900268324877));
#24094=CARTESIAN_POINT('Ctrl Pts',(15.,3.55239670909123,-1.43447068420923));
#24095=CARTESIAN_POINT('Ctrl Pts',(15.,3.590099835495,-1.31824322012931));
#24096=CARTESIAN_POINT('Ctrl Pts',(15.,3.62242629257587,-1.20074292158529));
#24097=CARTESIAN_POINT('Ctrl Pts',(15.,3.65467682719235,-1.08351858623173));
#24098=CARTESIAN_POINT('Ctrl Pts',(15.,3.68157610969259,-0.965026499777471));
#24099=CARTESIAN_POINT('Ctrl Pts',(15.,3.70297113528148,-0.845674315408051));
#24100=CARTESIAN_POINT('Ctrl Pts',(15.,3.72380182912614,-0.729470256573858));
#24101=CARTESIAN_POINT('Ctrl Pts',(15.,3.73941478911051,-0.612450092321461));
#24102=CARTESIAN_POINT('Ctrl Pts',(15.,3.74962026873843,-0.494990953545431));
#24103=CARTESIAN_POINT('Ctrl Pts',(15.,3.75681704041738,-0.412160294507659));
#24104=CARTESIAN_POINT('Ctrl Pts',(15.,3.76132374153974,-0.329111341532594));
#24105=CARTESIAN_POINT('Ctrl Pts',(15.,3.76305869017149,-0.245979715350486));
#24106=CARTESIAN_POINT('Ctrl Pts',(15.,3.76368445161509,-0.215995792220352));
#24107=CARTESIAN_POINT('Ctrl Pts',(15.,3.76394951400646,-0.186001152326826));
#24108=CARTESIAN_POINT('Ctrl Pts',(15.,3.76384962862183,-0.156002306664786));
#24109=CARTESIAN_POINT('Ctrl Pts',(15.,3.76378992941917,-0.138072684895765));
#24110=CARTESIAN_POINT('Ctrl Pts',(15.,3.76359976828237,-0.120140261775781));
#24111=CARTESIAN_POINT('Ctrl Pts',(15.,3.76327872654335,-0.102224379574802));
#24112=CARTESIAN_POINT('Ctrl Pts',(15.,3.7611762610886,0.0151046740680469));
#24113=CARTESIAN_POINT('Ctrl Pts',(15.,3.75346533085488,0.131899636400721));
#24114=CARTESIAN_POINT('Ctrl Pts',(15.,3.74000614617998,0.247789192086024));
#24115=CARTESIAN_POINT('Ctrl Pts',(15.,3.7303579680308,0.330864289567014));
#24116=CARTESIAN_POINT('Ctrl Pts',(15.,3.71775491296525,0.413474227796892));
#24117=CARTESIAN_POINT('Ctrl Pts',(15.,3.70212909055716,0.49547992626668));
#24118=CARTESIAN_POINT('Ctrl Pts',(15.,3.68014511871305,0.610853755504814));
#24119=CARTESIAN_POINT('Ctrl Pts',(15.,3.65217973575864,0.725032707578649));
#24120=CARTESIAN_POINT('Ctrl Pts',(15.,3.61851345531731,0.837703056235049));
#24121=CARTESIAN_POINT('Ctrl Pts',(15.,3.58455108518543,0.951364323051458));
#24122=CARTESIAN_POINT('Ctrl Pts',(15.,3.54478656262233,1.06349105917797));
#24123=CARTESIAN_POINT('Ctrl Pts',(15.,3.4994629109816,1.17373379051609));
#24124=CARTESIAN_POINT('Ctrl Pts',(15.,3.48735010956251,1.20319629550534));
#24125=CARTESIAN_POINT('Ctrl Pts',(15.,3.47484003581574,1.23252405453656));
#24126=CARTESIAN_POINT('Ctrl Pts',(15.,3.46193686781402,1.26170996577144));
#24127=CARTESIAN_POINT('Ctrl Pts',(15.,3.45526116077079,1.27680986938952));
#24128=CARTESIAN_POINT('Ctrl Pts',(15.,3.4484840071925,1.29186323438959));
#24129=CARTESIAN_POINT('Ctrl Pts',(15.,3.44160728857144,1.306867154827));
#24130=CARTESIAN_POINT('Ctrl Pts',(15.,3.39287914176642,1.41318432119845));
#24131=CARTESIAN_POINT('Ctrl Pts',(15.,3.3391404716466,1.51705536326108));
#24132=CARTESIAN_POINT('Ctrl Pts',(15.,3.2806979050605,1.61818973367994));
#24133=CARTESIAN_POINT('Ctrl Pts',(15.,3.22190782882257,1.7199254666314));
#24134=CARTESIAN_POINT('Ctrl Pts',(15.,3.15835716382197,1.81889257743335));
#24135=CARTESIAN_POINT('Ctrl Pts',(15.,3.09031245415742,1.91476797192053));
#24136=CARTESIAN_POINT('Ctrl Pts',(15.,3.02278563717085,2.0099136525909));
#24137=CARTESIAN_POINT('Ctrl Pts',(15.,2.95083228311762,2.10201510480185));
#24138=CARTESIAN_POINT('Ctrl Pts',(15.,2.87467744809909,2.19072013381056));
#24139=CARTESIAN_POINT('Ctrl Pts',(15.,2.82842890210364,2.24459036559741));
#24140=CARTESIAN_POINT('Ctrl Pts',(15.,2.78063016774874,2.29720722102989));
#24141=CARTESIAN_POINT('Ctrl Pts',(15.,2.73132668700375,2.34848374369048));
#24142=CARTESIAN_POINT('Ctrl Pts',(15.,2.71416029468208,2.36633710600045));
#24143=CARTESIAN_POINT('Ctrl Pts',(15.,2.69681145622203,2.384027923152));
#24144=CARTESIAN_POINT('Ctrl Pts',(15.,2.67928200313545,2.40155232826184));
#24145=CARTESIAN_POINT('Ctrl Pts',(15.,2.66457020727519,2.41625988754935));
#24146=CARTESIAN_POINT('Ctrl Pts',(15.,2.64972855828448,2.43085265888608));
#24147=CARTESIAN_POINT('Ctrl Pts',(15.,2.63477716327216,2.44531024066103));
#24148=CARTESIAN_POINT('Ctrl Pts',(15.,2.55170266149999,2.52564096577364));
#24149=CARTESIAN_POINT('Ctrl Pts',(15.,2.46513368308695,2.60191292355531));
#24150=CARTESIAN_POINT('Ctrl Pts',(15.,2.37532241430713,2.67382459269717));
#24151=CARTESIAN_POINT('Ctrl Pts',(15.,2.28654836265619,2.74490576455274));
#24152=CARTESIAN_POINT('Ctrl Pts',(15.,2.19460584593852,2.81172729121945));
#24153=CARTESIAN_POINT('Ctrl Pts',(15.,2.09970897870241,2.87395745757045));
#24154=CARTESIAN_POINT('Ctrl Pts',(15.,2.00713664782224,2.93466327134448));
#24155=CARTESIAN_POINT('Ctrl Pts',(15.,1.91175234806588,2.9910002513087));
#24156=CARTESIAN_POINT('Ctrl Pts',(15.,1.81373561196281,3.04261555880697));
#24157=CARTESIAN_POINT('Ctrl Pts',(15.,1.71571887585974,3.09423086630524));
#24158=CARTESIAN_POINT('Ctrl Pts',(15.,1.61506922876594,3.14112502559283));
#24159=CARTESIAN_POINT('Ctrl Pts',(15.,1.51195443948848,3.18289299779479));
#24160=CARTESIAN_POINT('Ctrl Pts',(15.,-2.52120044613813,2.46936361140965));
#24161=CARTESIAN_POINT('Ctrl Pts',(15.,-2.60179898682872,2.39717859433151));
#24162=CARTESIAN_POINT('Ctrl Pts',(15.,-2.67869877568603,2.3212580895175));
#24163=CARTESIAN_POINT('Ctrl Pts',(15.,-2.75155631737188,2.24172753651207));
#24164=CARTESIAN_POINT('Ctrl Pts',(15.,-2.82661178723241,2.15979774741999));
#24165=CARTESIAN_POINT('Ctrl Pts',(15.,-2.8973785762359,2.07403697418862));
#24166=CARTESIAN_POINT('Ctrl Pts',(15.,-2.96383857017409,1.98486101330688));
#24167=CARTESIAN_POINT('Ctrl Pts',(15.,-3.00474733706439,1.92996966620079));
#24168=CARTESIAN_POINT('Ctrl Pts',(15.,-3.04402362867714,1.87378350573605));
#24169=CARTESIAN_POINT('Ctrl Pts',(15.,-3.08165627846039,1.81639284598983));
#24170=CARTESIAN_POINT('Ctrl Pts',(15.,-3.09368658503351,1.79804635072156));
#24171=CARTESIAN_POINT('Ctrl Pts',(15.,-3.10554887976004,1.77957672978204));
#24172=CARTESIAN_POINT('Ctrl Pts',(15.,-3.11724267731674,1.76098684436662));
#24173=CARTESIAN_POINT('Ctrl Pts',(15.,-3.12837591079725,1.74328809990809));
#24174=CARTESIAN_POINT('Ctrl Pts',(15.,-3.1393524148385,1.72548662453293));
#24175=CARTESIAN_POINT('Ctrl Pts',(15.,-3.15016852685405,1.70759114823924));
#24176=CARTESIAN_POINT('Ctrl Pts',(15.,-3.20879801673494,1.61058747032193));
#24177=CARTESIAN_POINT('Ctrl Pts',(15.,-3.2627518772499,1.51077072777429));
#24178=CARTESIAN_POINT('Ctrl Pts',(15.,-3.31201510422133,1.40857225843896));
#24179=CARTESIAN_POINT('Ctrl Pts',(15.,-3.35951680124557,1.31002815109649));
#24180=CARTESIAN_POINT('Ctrl Pts',(15.,-3.40265730316664,1.20926876756575));
#24181=CARTESIAN_POINT('Ctrl Pts',(15.,-3.44138896342653,1.10665322186668));
#24182=CARTESIAN_POINT('Ctrl Pts',(15.,-3.45833406479024,1.06175892062334));
#24183=CARTESIAN_POINT('Ctrl Pts',(15.,-3.47443483618565,1.01650904659998));
#24184=CARTESIAN_POINT('Ctrl Pts',(15.,-3.48968512212765,0.970932519453672));
#24185=CARTESIAN_POINT('Ctrl Pts',(15.,-3.4983119898275,0.945150532715522));
#24186=CARTESIAN_POINT('Ctrl Pts',(15.,-3.50666667748744,0.91926400607298));
#24187=CARTESIAN_POINT('Ctrl Pts',(15.,-3.51474787552058,0.893278102137526));
#24188=CARTESIAN_POINT('Ctrl Pts',(15.,-3.52046912920241,0.874880836291959));
#24189=CARTESIAN_POINT('Ctrl Pts',(15.,-3.52605061516273,0.856442309316086));
#24190=CARTESIAN_POINT('Ctrl Pts',(15.,-3.53149085344976,0.837969346152265));
#24191=CARTESIAN_POINT('Ctrl Pts',(15.,-3.56477303826427,0.724955808573256));
#24192=CARTESIAN_POINT('Ctrl Pts',(15.,-3.59279001212681,0.610598793555419));
#24193=CARTESIAN_POINT('Ctrl Pts',(15.,-3.61551923482663,0.495347390597081));
#24194=CARTESIAN_POINT('Ctrl Pts',(15.,-3.63850038450621,0.378818559974632));
#24195=CARTESIAN_POINT('Ctrl Pts',(15.,-3.65607624651716,0.261374564334388));
#24196=CARTESIAN_POINT('Ctrl Pts',(15.,-3.66817706892989,0.14345385470107));
#24197=CARTESIAN_POINT('Ctrl Pts',(15.,-3.68015016445688,0.0267778245194678));
#24198=CARTESIAN_POINT('Ctrl Pts',(15.,-3.68676336140009,-0.0903658031962653));
#24199=CARTESIAN_POINT('Ctrl Pts',(15.,-3.68790038379689,-0.207564280302668));
#24200=CARTESIAN_POINT('Ctrl Pts',(15.,-3.68867220478621,-0.287119656521374));
#24201=CARTESIAN_POINT('Ctrl Pts',(15.,-3.68691970242156,-0.366700546990979));
#24202=CARTESIAN_POINT('Ctrl Pts',(15.,-3.68259285188237,-0.446177887149181));
#24203=CARTESIAN_POINT('Ctrl Pts',(15.,-3.68144217396426,-0.467314004396978));
#24204=CARTESIAN_POINT('Ctrl Pts',(15.,-3.68010936634767,-0.488442791064557));
#24205=CARTESIAN_POINT('Ctrl Pts',(15.,-3.67859335009362,-0.509561799177698));
#24206=CARTESIAN_POINT('Ctrl Pts',(15.,-3.67741985285778,-0.525909313644376));
#24207=CARTESIAN_POINT('Ctrl Pts',(15.,-3.67613653785577,-0.542250677006092));
#24208=CARTESIAN_POINT('Ctrl Pts',(15.,-3.67474426482348,-0.558570866196314));
#24209=CARTESIAN_POINT('Ctrl Pts',(15.,-3.66454291715474,-0.67815080496419));
#24210=CARTESIAN_POINT('Ctrl Pts',(15.,-3.64848322229041,-0.796782907711174));
#24211=CARTESIAN_POINT('Ctrl Pts',(15.,-3.62650052051321,-0.914027217005267));
#24212=CARTESIAN_POINT('Ctrl Pts',(15.,-3.61163636836508,-0.993304881302997));
#24213=CARTESIAN_POINT('Ctrl Pts',(15.,-3.59406313593742,-1.07194840668789));
#24214=CARTESIAN_POINT('Ctrl Pts',(15.,-3.57374739672799,-1.14982341224806));
#24215=CARTESIAN_POINT('Ctrl Pts',(15.,-3.54447892467199,-1.26201634801092));
#24216=CARTESIAN_POINT('Ctrl Pts',(15.,-3.50952067095247,-1.37261494887389));
#24217=CARTESIAN_POINT('Ctrl Pts',(15.,-3.46919598978005,-1.48138234197029));
#24218=CARTESIAN_POINT('Ctrl Pts',(15.,-3.42815857585037,-1.59207218260321));
#24219=CARTESIAN_POINT('Ctrl Pts',(15.,-3.38156301779153,-1.70086616239473));
#24220=CARTESIAN_POINT('Ctrl Pts',(15.,-3.32969852456671,-1.80749900795472));
#24221=CARTESIAN_POINT('Ctrl Pts',(15.,-3.31675311277751,-1.8341146366864));
#24222=CARTESIAN_POINT('Ctrl Pts',(15.,-3.30347921086797,-1.86059552333069));
#24223=CARTESIAN_POINT('Ctrl Pts',(15.,-3.28988086646955,-1.8869373191648));
#24224=CARTESIAN_POINT('Ctrl Pts',(15.,-3.28041699897394,-1.90527008513));
#24225=CARTESIAN_POINT('Ctrl Pts',(15.,-3.27079458652134,-1.92353788999526));
#24226=CARTESIAN_POINT('Ctrl Pts',(15.,-3.26102676821148,-1.94171779428929));
#24227=CARTESIAN_POINT('Ctrl Pts',(15.,-3.2023945117954,-2.05084439517136));
#24228=CARTESIAN_POINT('Ctrl Pts',(15.,-3.13844653177481,-2.15696706986354));
#24229=CARTESIAN_POINT('Ctrl Pts',(15.,-3.06959759380989,-2.25981885873531));
#24230=CARTESIAN_POINT('Ctrl Pts',(15.,-3.00218015142085,-2.36053217045558));
#24231=CARTESIAN_POINT('Ctrl Pts',(15.,-2.93006266448803,-2.45810980071153));
#24232=CARTESIAN_POINT('Ctrl Pts',(15.,-2.85358047685615,-2.5522851851895));
#24233=CARTESIAN_POINT('Ctrl Pts',(15.,-2.77668643075426,-2.64696770643963));
#24234=CARTESIAN_POINT('Ctrl Pts',(15.,-2.69538003166737,-2.73821192706575));
#24235=CARTESIAN_POINT('Ctrl Pts',(15.,-2.60995605577262,-2.82572098699874));
#24236=CARTESIAN_POINT('Ctrl Pts',(15.,-2.55533062672409,-2.88167974909572));
#24237=CARTESIAN_POINT('Ctrl Pts',(15.,-2.49902056538751,-2.93611060646992));
#24238=CARTESIAN_POINT('Ctrl Pts',(15.,-2.44109466904705,-2.98892841607831));
#24239=CARTESIAN_POINT('Ctrl Pts',(15.,-2.41749244372008,-3.01044932334795));
#24240=CARTESIAN_POINT('Ctrl Pts',(15.,-2.39362188975801,-3.03170235637655));
#24241=CARTESIAN_POINT('Ctrl Pts',(15.,-2.36948739594367,-3.0526814236989));
#24242=CARTESIAN_POINT('Ctrl Pts',(15.,-2.35462633600607,-3.06559949769335));
#24243=CARTESIAN_POINT('Ctrl Pts',(15.,-2.33966395888483,-3.07841463134345));
#24244=CARTESIAN_POINT('Ctrl Pts',(15.,-2.32461750573873,-3.09111197026854));
#24245=CARTESIAN_POINT('Ctrl Pts',(15.,-2.2294342138806,-3.17143485467153));
#24246=CARTESIAN_POINT('Ctrl Pts',(15.,-2.1307475718697,-3.24717166060831));
#24247=CARTESIAN_POINT('Ctrl Pts',(15.,-2.02890261537899,-3.31805078240874));
#24248=CARTESIAN_POINT('Ctrl Pts',(15.,-1.92724043909641,-3.38880269810018));
#24249=CARTESIAN_POINT('Ctrl Pts',(15.,-1.82243067018098,-3.45471500591087));
#24250=CARTESIAN_POINT('Ctrl Pts',(15.,-1.71477564167398,-3.51548571648839));
#24251=CARTESIAN_POINT('Ctrl Pts',(15.,-1.6070666174637,-3.57628690736305));
#24252=CARTESIAN_POINT('Ctrl Pts',(15.,-1.49650889611397,-3.63194202719247));
#24253=CARTESIAN_POINT('Ctrl Pts',(15.,-1.38337320787942,-3.68210666696541));
#24254=CARTESIAN_POINT('Ctrl Pts',(15.,-1.27023751964487,-3.73227130673836));
#24255=CARTESIAN_POINT('Ctrl Pts',(15.,-1.15452327651166,-3.77694617659555));
#24256=CARTESIAN_POINT('Ctrl Pts',(15.,-1.03647793659398,-3.81573446232228));
#24257=CARTESIAN_POINT('Ctrl Pts',(-5.89440495331884,-1.50460803346933,
3.1863723461202));
#24258=CARTESIAN_POINT('Ctrl Pts',(-5.85483221666482,-2.56096624880367,
2.6875589984119));
#24259=CARTESIAN_POINT('Ctrl Pts',(-5.7756867433568,-4.12083736250477,0.565882107592299));
#24260=CARTESIAN_POINT('Ctrl Pts',(-5.65696853339476,-2.71711677464747,
-3.15455318962618));
#24261=CARTESIAN_POINT('Ctrl Pts',(-5.53825032343272,1.16346364900644,-3.99342346061016));
#24262=CARTESIAN_POINT('Ctrl Pts',(-5.41953211347069,3.98315669070171,-1.20222141896168));
#24263=CARTESIAN_POINT('Ctrl Pts',(-5.30081390350864,3.17803017110567,2.68595570733295));
#24264=CARTESIAN_POINT('Ctrl Pts',(-5.18209569354661,-0.520477180563039,
4.12779813317261));
#24265=CARTESIAN_POINT('Ctrl Pts',(-5.06337748358456,-3.74494492974617,
1.81293102525157));
#24266=CARTESIAN_POINT('Ctrl Pts',(-4.94465927362253,-3.56061979352912,
-2.1525824195332));
#24267=CARTESIAN_POINT('Ctrl Pts',(-4.82594106366048,-0.135078114281208,
-4.15845351012906));
#24268=CARTESIAN_POINT('Ctrl Pts',(-4.70722285369845,3.41338373023632,-2.37909235958642));
#24269=CARTESIAN_POINT('Ctrl Pts',(-4.58850464373641,3.85474686870501,1.56595294230416));
#24270=CARTESIAN_POINT('Ctrl Pts',(-4.46978643377438,0.787218792347394,
4.08552098175258));
#24271=CARTESIAN_POINT('Ctrl Pts',(-4.35106822381233,-2.99688953094326,
2.88615565105121));
#24272=CARTESIAN_POINT('Ctrl Pts',(-4.2323500138503,-4.05300639018084,-0.940413777248205));
#24273=CARTESIAN_POINT('Ctrl Pts',(-4.11363180388825,-1.41977030063975,
-3.9109435932429));
#24274=CARTESIAN_POINT('Ctrl Pts',(-3.99491359392623,2.50584675349696,-3.32144046072034));
#24275=CARTESIAN_POINT('Ctrl Pts',(-3.87619538396417,4.1504539432636,0.29148889536334));
#24276=CARTESIAN_POINT('Ctrl Pts',(-3.75747717400214,2.01700539684609,3.63908250952178));
#24277=CARTESIAN_POINT('Ctrl Pts',(-3.6387589640401,-1.9524731306016,3.67410969416408));
#24278=CARTESIAN_POINT('Ctrl Pts',(-3.52004075407806,-4.14466374650587,
0.364685577384703));
#24279=CARTESIAN_POINT('Ctrl Pts',(-3.40132254411603,-2.56406948928158,
-3.2767027063953));
#24280=CARTESIAN_POINT('Ctrl Pts',(-3.28260433415398,1.35053375419133,-3.93538965177946));
#24281=CARTESIAN_POINT('Ctrl Pts',(-3.16388612419195,4.03577955172485,-1.0117887612591));
#24282=CARTESIAN_POINT('Ctrl Pts',(-3.0451679142299,3.04735509174485,2.83281838700313));
#24283=CARTESIAN_POINT('Ctrl Pts',(-2.92644970426787,-0.715001293115481,
4.09878106793642));
#24284=CARTESIAN_POINT('Ctrl Pts',(-2.80773149430582,-3.82650969623519,
1.63372477135958));
#24285=CARTESIAN_POINT('Ctrl Pts',(-2.68901328434379,-3.4548410165288,-2.31847075303888));
#24286=CARTESIAN_POINT('Ctrl Pts',(-2.57029507438175,0.0616839434797912,
-4.16021972695477));
#24287=CARTESIAN_POINT('Ctrl Pts',(-2.45157686441971,3.52205953641558,-2.21502363553932));
#24288=CARTESIAN_POINT('Ctrl Pts',(-2.33285865445767,3.77639149338881,1.74645365601417));
#24289=CARTESIAN_POINT('Ctrl Pts',(-2.21414044449563,0.593167728051762,
4.11817740399618));
#24290=CARTESIAN_POINT('Ctrl Pts',(-2.09542223453359,-3.13000194108223,
2.74122617326354));
#24291=CARTESIAN_POINT('Ctrl Pts',(-1.97670402457155,-4.00400830115146,
-1.13099540603816));
#24292=CARTESIAN_POINT('Ctrl Pts',(-1.85798581460952,-1.233264991575,-3.97369985590045));
#24293=CARTESIAN_POINT('Ctrl Pts',(-1.73926760464748,2.66008892032246,-3.19924366376966));
#24294=CARTESIAN_POINT('Ctrl Pts',(-1.62054939468544,4.13202971706382,0.487404864048419));
#24295=CARTESIAN_POINT('Ctrl Pts',(-1.5018311847234,1.8426861173841,3.73038080589689));
#24296=CARTESIAN_POINT('Ctrl Pts',(-1.38311297476136,-2.12400905413959,
3.57768341558217));
#24297=CARTESIAN_POINT('Ctrl Pts',(-1.26439476479932,-4.1572713463681,0.168309348719648));
#24298=CARTESIAN_POINT('Ctrl Pts',(-1.14567655483728,-2.40627241167155,
-3.39427255314433));
#24299=CARTESIAN_POINT('Ctrl Pts',(-1.02695834487524,1.53509675153174,-3.86713214768211));
#24300=CARTESIAN_POINT('Ctrl Pts',(-0.908240134913205,4.07910533073667,
-0.819837047806264));
#24301=CARTESIAN_POINT('Ctrl Pts',(-0.789521924951166,2.91000527267733,
2.97373542824345));
#24302=CARTESIAN_POINT('Ctrl Pts',(-0.670803714989128,-0.908000571423945,
4.06039013476461));
#24303=CARTESIAN_POINT('Ctrl Pts',(-0.552085505027088,-3.89947596557817,
1.45097218377135));
#24304=CARTESIAN_POINT('Ctrl Pts',(-0.43336729506505,-3.34135488829783,
-2.47922983901215));
#24305=CARTESIAN_POINT('Ctrl Pts',(-0.31464908510301,0.258318855548078,
-4.15265029265267));
#24306=CARTESIAN_POINT('Ctrl Pts',(-0.195930875140972,3.62285133778538,
-2.04601595020828));
#24307=CARTESIAN_POINT('Ctrl Pts',(-0.0772126651789335,3.68959190165954,
1.92305607911166));
#24308=CARTESIAN_POINT('Ctrl Pts',(0.0415055447831062,0.397788263499511,
4.14161774933685));
#24309=CARTESIAN_POINT('Ctrl Pts',(0.160223754745144,-3.25611218688863,
2.59016727463602));
#24310=CARTESIAN_POINT('Ctrl Pts',(0.278941964707183,-3.94605429230943,
-1.31904837149603));
#24311=CARTESIAN_POINT('Ctrl Pts',(0.397660174669222,-1.04400082814246,
-4.02756692744365));
#24312=CARTESIAN_POINT('Ctrl Pts',(0.516378384631262,2.80838075407454,-3.06989097922772));
#24313=CARTESIAN_POINT('Ctrl Pts',(0.635096594593299,4.10436283463961,0.682230757023696));
#24314=CARTESIAN_POINT('Ctrl Pts',(0.75381480455534,1.66424499718303,3.81333471826842));
#24315=CARTESIAN_POINT('Ctrl Pts',(0.872533014517378,-2.29079387626655,
3.47325445377382));
#24316=CARTESIAN_POINT('Ctrl Pts',(0.991251224479415,-4.16057977425022,
-0.0284433876307468));
#24317=CARTESIAN_POINT('Ctrl Pts',(1.10996943444146,-2.24309286528101,-3.50424991716136));
#24318=CARTESIAN_POINT('Ctrl Pts',(1.22868764440349,1.71622596930723,-3.79022446650269));
#24319=CARTESIAN_POINT('Ctrl Pts',(1.34740585436554,4.11330677534691,-0.626051480379392));
#24320=CARTESIAN_POINT('Ctrl Pts',(1.46612406432757,2.7661462154741,3.10800067548548));
#24321=CARTESIAN_POINT('Ctrl Pts',(1.58484227428961,-1.09896879073751,4.01291672990917));
#24322=CARTESIAN_POINT('Ctrl Pts',(1.70356048425165,-3.96371970283678,1.26497399243763));
#24323=CARTESIAN_POINT('Ctrl Pts',(1.82227869421369,-3.22039465930975,-2.63444326613598));
#24324=CARTESIAN_POINT('Ctrl Pts',(1.94099690417573,0.454375947728439,-4.13579201391049));
#24325=CARTESIAN_POINT('Ctrl Pts',(2.05971511413777,3.71553937395602,-1.87243163954858));
#24326=CARTESIAN_POINT('Ctrl Pts',(2.17843332409981,3.594539256238,2.09535691937294));
#24327=CARTESIAN_POINT('Ctrl Pts',(2.29715153406184,0.201519007352503,4.15579392822546));
#24328=CARTESIAN_POINT('Ctrl Pts',(2.41586974402388,-3.37493900695059,2.43331456732649));
#24329=CARTESIAN_POINT('Ctrl Pts',(2.53458795398592,-3.87927356258216,-1.5041508271617));
#24330=CARTESIAN_POINT('Ctrl Pts',(2.65330616394796,-0.852401394279078,
-4.07242494678922));
#24331=CARTESIAN_POINT('Ctrl Pts',(2.77202437391,2.95039066892461,-2.93367141734082));
#24332=CARTESIAN_POINT('Ctrl Pts',(2.89074258387204,4.06751511929676,0.875530603972367));
#24333=CARTESIAN_POINT('Ctrl Pts',(3.00946079383408,1.48208121505632,3.88775878317795));
#24334=CARTESIAN_POINT('Ctrl Pts',(3.12817900379612,-2.45245454230029,3.36105635212366));
#24335=CARTESIAN_POINT('Ctrl Pts',(3.24689721375816,-4.1545816205045,-0.225132500466264));
#24336=CARTESIAN_POINT('Ctrl Pts',(3.3656154237202,-2.07489586267471,-3.60638880921834));
#24337=CARTESIAN_POINT('Ctrl Pts',(3.48433363368223,1.89351625165984,-3.70483863196498));
#24338=CARTESIAN_POINT('Ctrl Pts',(3.60305184364428,4.13830738080923,-0.430865531390001));
#24339=CARTESIAN_POINT('Ctrl Pts',(3.72177005360631,2.6160997115818,3.23531379981317));
#24340=CARTESIAN_POINT('Ctrl Pts',(3.84048826356835,-1.28747878468051,3.95646704310772));
#24341=CARTESIAN_POINT('Ctrl Pts',(3.95920647353038,-4.01909720438648,1.07614624744637));
#24342=CARTESIAN_POINT('Ctrl Pts',(4.07792468349243,-3.09223089922823,-2.78376384595717));
#24343=CARTESIAN_POINT('Ctrl Pts',(4.19664289345446,0.649416670297701,-4.10968259997526));
#24344=CARTESIAN_POINT('Ctrl Pts',(4.3153611034165,3.79991631591589,-1.69465898523452));
#24345=CARTESIAN_POINT('Ctrl Pts',(4.43407931337854,3.49144617539216,2.26297076616989));
#24346=CARTESIAN_POINT('Ctrl Pts',(4.55279752334059,0.00479898395836184,
4.16067423069304));
#24347=CARTESIAN_POINT('Ctrl Pts',(4.67151573330262,-3.48621660381262,2.27101890690085));
#24348=CARTESIAN_POINT('Ctrl Pts',(4.79023394326466,-3.80381549026664,-1.68588872711323));
#24349=CARTESIAN_POINT('Ctrl Pts',(4.90895215322669,-0.658895268659781,
-4.10817357339461));
#24350=CARTESIAN_POINT('Ctrl Pts',(5.02767036318875,3.08580101037766,-2.79088968046971));
#24351=CARTESIAN_POINT('Ctrl Pts',(5.14638857315077,4.02156899374811,1.06687202265491));
#24352=CARTESIAN_POINT('Ctrl Pts',(5.26510678311282,1.29660224356769,3.95348652535647));
#24353=CARTESIAN_POINT('Ctrl Pts',(5.38382499307485,-2.60862944201661,3.24134008065248));
#24354=CARTESIAN_POINT('Ctrl Pts',(5.5025432030369,-4.13929030208498,-0.421318026276293));
#24355=CARTESIAN_POINT('Ctrl Pts',(5.62126141299893,-1.90205763486351,-3.70046076021046));
#24356=CARTESIAN_POINT('Ctrl Pts',(5.73997962296098,2.06657102730044,-3.61116563914235));
#24357=CARTESIAN_POINT('Ctrl Pts',(5.85869783292301,4.15405122458681,-0.23471580200077));
#24358=CARTESIAN_POINT('Ctrl Pts',(5.97741604288506,2.46020139211735,3.35539002120827));
#24359=CARTESIAN_POINT('Ctrl Pts',(6.09613425284709,-1.47310888518228,3.89116734368968));
#24360=CARTESIAN_POINT('Ctrl Pts',(6.21485246280913,-4.06548459921251,0.884911327628835));
#24361=CARTESIAN_POINT('Ctrl Pts',(6.33357067277116,-2.95715029081375,-2.92685757114013));
#24362=CARTESIAN_POINT('Ctrl Pts',(6.45228888273322,0.843004746942437,-4.07438045361901));
#24363=CARTESIAN_POINT('Ctrl Pts',(6.57100709269524,3.87579342533039,-1.51309563754761));
#24364=CARTESIAN_POINT('Ctrl Pts',(6.68972530265728,3.38054326260136,2.42552269292219));
#24365=CARTESIAN_POINT('Ctrl Pts',(6.80844351261932,-0.191931774030066,
4.15624774024814));
#24366=CARTESIAN_POINT('Ctrl Pts',(6.92716172258136,-3.58969606648277,2.10364332396875));
#24367=CARTESIAN_POINT('Ctrl Pts',(7.0458799325434,-3.71984886354811,-1.86385555142016));
#24368=CARTESIAN_POINT('Ctrl Pts',(7.16459814250543,-0.463915294938845,
-4.13473284304098));
#24369=CARTESIAN_POINT('Ctrl Pts',(7.28331635246748,3.21430888617722,-2.64186514955669));
#24370=CARTESIAN_POINT('Ctrl Pts',(7.40203456242951,3.96662723246049,1.25582701153581));
#24371=CARTESIAN_POINT('Ctrl Pts',(7.52075277239156,1.1082229708534,4.01037092188151));
#24372=CARTESIAN_POINT('Ctrl Pts',(7.63947098235359,-2.75896923601302,3.11437342637868));
#24373=CARTESIAN_POINT('Ctrl Pts',(7.75818919231563,-4.11474002333594,-0.61656112799747));
#24374=CARTESIAN_POINT('Ctrl Pts',(7.87690740227768,-1.7249647945704,-3.78625534554826));
#24375=CARTESIAN_POINT('Ctrl Pts',(7.9956256122397,2.2350031991217,-3.50941502021571));
#24376=CARTESIAN_POINT('Ctrl Pts',(8.11434382220176,4.16050309010526,-0.0380410492039316));
#24377=CARTESIAN_POINT('Ctrl Pts',(8.23306203216378,2.2987999778154,3.46796074749932));
#24378=CARTESIAN_POINT('Ctrl Pts',(8.35178024212583,-1.65544386605393,3.81716369711131));
#24379=CARTESIAN_POINT('Ctrl Pts',(8.47049845208786,-4.10277812579614,0.691696996298736));
#24380=CARTESIAN_POINT('Ctrl Pts',(8.5892166620499,-2.81545498876027,-3.06340436287227));
#24381=CARTESIAN_POINT('Ctrl Pts',(8.70793487201195,1.03470715069641,-4.02996454035241));
#24382=CARTESIAN_POINT('Ctrl Pts',(8.82665308197397,3.9430009766923,-1.32814772597166));
#24383=CARTESIAN_POINT('Ctrl Pts',(8.94537129193603,3.26207859074647,2.58264909579165));
#24384=CARTESIAN_POINT('Ctrl Pts',(9.06408950189805,-0.388233209948286,
4.14252435827397));
#24385=CARTESIAN_POINT('Ctrl Pts',(9.1828077118601,-3.68514592720451,1.93156221215062));
#24386=CARTESIAN_POINT('Ctrl Pts',(9.30152592182213,-3.62756150294873,-2.03765321547226));
#24387=CARTESIAN_POINT('Ctrl Pts',(9.42024413178417,-0.267897613543705,
-4.1520433466978));
#24388=CARTESIAN_POINT('Ctrl Pts',(9.53896234174623,3.33562684382852,-2.48693116972114));
#24389=CARTESIAN_POINT('Ctrl Pts',(9.65768055170824,3.90281273176416,1.44197290715868));
#24390=CARTESIAN_POINT('Ctrl Pts',(9.77639876167031,0.917364772580788,4.05828473104436));
#24391=CARTESIAN_POINT('Ctrl Pts',(9.89511697163233,-2.90313763712753,2.98044039431988));
#24392=CARTESIAN_POINT('Ctrl Pts',(10.0138351815944,-4.08098569948204,-0.810425076625216));
#24393=CARTESIAN_POINT('Ctrl Pts',(10.1325533915564,-1.54401347143674,-3.86358065584526));
#24394=CARTESIAN_POINT('Ctrl Pts',(10.2512716015185,2.3984360100751,-3.39981437578226));
#24395=CARTESIAN_POINT('Ctrl Pts',(10.3699898114805,4.15764854552659,0.158718795611215));
#24396=CARTESIAN_POINT('Ctrl Pts',(10.4887080214425,2.13225649899359,3.57277417516111));
#24397=CARTESIAN_POINT('Ctrl Pts',(10.6074262314046,-1.83407587178631,3.73462163822996));
#24398=CARTESIAN_POINT('Ctrl Pts',(10.7261444413666,-4.13089436421284,0.496935444410325));
#24399=CARTESIAN_POINT('Ctrl Pts',(10.8448626513286,-2.66746194382199,-3.1930987868298));
#24400=CARTESIAN_POINT('Ctrl Pts',(10.9635808612907,1.22409507255686,-3.97653421179419));
#24401=CARTESIAN_POINT('Ctrl Pts',(11.0822990712527,4.00138863696973,-1.14022895073704));
#24402=CARTESIAN_POINT('Ctrl Pts',(11.2010172812148,3.13631714721284,2.73399850699711));
#24403=CARTESIAN_POINT('Ctrl Pts',(11.3197354911768,-0.583666227467498,
4.11953478190202));
#24404=CARTESIAN_POINT('Ctrl Pts',(11.4384537011388,-3.77235267919998,1.75516049057551));
#24405=CARTESIAN_POINT('Ctrl Pts',(11.5571719111009,-3.52715984122978,-2.20689296035622));
#24406=CARTESIAN_POINT('Ctrl Pts',(11.6758901210629,-0.071280686042087,
-4.16006636356011));
#24407=CARTESIAN_POINT('Ctrl Pts',(11.7946083310249,3.44948351348419,-2.32643430433509));
#24408=CARTESIAN_POINT('Ctrl Pts',(11.913326540987,3.83026823514579,1.62489332904317));
#24409=CARTESIAN_POINT('Ctrl Pts',(12.032044750949,0.724454569027592,4.09712077799104));
#24410=CARTESIAN_POINT('Ctrl Pts',(12.1507629609111,-3.04081216196281,2.83984057027597));
#24411=CARTESIAN_POINT('Ctrl Pts',(12.2694811708731,-4.03810283512032,-1.00247622441819));
#24412=CARTESIAN_POINT('Ctrl Pts',(12.3881993808351,-1.35960842341351,-3.93226373321093));
#24413=CARTESIAN_POINT('Ctrl Pts',(12.5069175907972,2.55650388111248,-3.28260885239469));
#24414=CARTESIAN_POINT('Ctrl Pts',(12.6256358007592,4.14549398517236,0.355123585322626));
#24415=CARTESIAN_POINT('Ctrl Pts',(12.7443540107213,1.96094347059736,3.66959590085791));
#24416=CARTESIAN_POINT('Ctrl Pts',(12.8630722206833,-2.008605296796,3.64372570917414));
#24417=CARTESIAN_POINT('Ctrl Pts',(12.9817904306453,-4.14977048561323,0.301062498504729));
#24418=CARTESIAN_POINT('Ctrl Pts',(13.1005086406074,-2.51350207424876,-3.31565106862418));
#24419=CARTESIAN_POINT('Ctrl Pts',(13.2192268505694,1.41074465321508,-3.91420835157396));
#24420=CARTESIAN_POINT('Ctrl Pts',(13.3379450605315,4.05082623445229,-0.949760859141879));
#24421=CARTESIAN_POINT('Ctrl Pts',(13.4566632704935,3.00353941846475,2.8792346664523));
#24422=CARTESIAN_POINT('Ctrl Pts',(13.5753814804555,-0.777792108158467,
4.08732608875924));
#24423=CARTESIAN_POINT('Ctrl Pts',(13.6940996904176,-3.85112422993177,1.57484100941476));
#24424=CARTESIAN_POINT('Ctrl Pts',(13.8128179003796,-3.4188628023499,-2.37121194413166));
#24425=CARTESIAN_POINT('Ctrl Pts',(13.9315361103417,0.125484922544878,-4.15875404743734));
#24426=CARTESIAN_POINT('Ctrl Pts',(14.0502543203037,3.55564468470245,-2.16079042553925));
#24427=CARTESIAN_POINT('Ctrl Pts',(14.1689725302657,3.74911708348173,1.80428726191164));
#24428=CARTESIAN_POINT('Ctrl Pts',(14.2876907402278,0.529997911397081,4.12658649947203));
#24429=CARTESIAN_POINT('Ctrl Pts',(14.4064089501898,-3.1718256804096,2.69327972615298));
#24430=CARTESIAN_POINT('Ctrl Pts',(14.5251271601518,-3.98591940928569,-1.19302976726136));
#24431=CARTESIAN_POINT('Ctrl Pts',(14.6438453701139,-1.17267268992146,-3.99072892597622));
#24432=CARTESIAN_POINT('Ctrl Pts',(14.7625635800759,2.70983253704952,-3.16081271422384));
#24433=CARTESIAN_POINT('Ctrl Pts',(14.881281790038,4.12213179013054,0.556374543543842));
#24434=CARTESIAN_POINT('Ctrl Pts',(14.960427263346,2.56715916810242,2.68164414176901));
#24435=CARTESIAN_POINT('Ctrl Pts',(15.,1.51195443948848,3.18289299779479));
#24436=CARTESIAN_POINT('Ctrl Pts',(-5.81160330221256,-1.56584559822282,
3.31605773828462));
#24437=CARTESIAN_POINT('Ctrl Pts',(-5.77203056555855,-2.66519760541219,
2.79694268142636));
#24438=CARTESIAN_POINT('Ctrl Pts',(-5.69288509225052,-4.28855549188565,
0.588913516062578));
#24439=CARTESIAN_POINT('Ctrl Pts',(-5.57416688228849,-2.82770345950423,
-3.28294354174507));
#24440=CARTESIAN_POINT('Ctrl Pts',(-5.45544867232644,1.21081663327842,-4.15595584267732));
#24441=CARTESIAN_POINT('Ctrl Pts',(-5.33673046236441,4.1452712151122,-1.2511518449291));
#24442=CARTESIAN_POINT('Ctrl Pts',(-5.21801225240236,3.30737603664836,2.79527413638156));
#24443=CARTESIAN_POINT('Ctrl Pts',(-5.09929404244033,-0.541660607966363,
4.29579956600198));
#24444=CARTESIAN_POINT('Ctrl Pts',(-4.98057583247828,-3.89736423266904,
1.88671733941634));
#24445=CARTESIAN_POINT('Ctrl Pts',(-4.86185762251625,-3.70553706122838,
-2.24019254946148));
#24446=CARTESIAN_POINT('Ctrl Pts',(-4.74313941255421,-0.140575795129675,
-4.32770261716304));
#24447=CARTESIAN_POINT('Ctrl Pts',(-4.62442120259217,3.55230848841859,-2.47592144675321));
#24448=CARTESIAN_POINT('Ctrl Pts',(-4.50570299263013,4.01163511184185,1.6296872455726));
#24449=CARTESIAN_POINT('Ctrl Pts',(-4.3869847826681,0.819258606504406,4.25180173401925));
#24450=CARTESIAN_POINT('Ctrl Pts',(-4.26826657270605,-3.11886297028946,
3.0036222201764));
#24451=CARTESIAN_POINT('Ctrl Pts',(-4.14954836274402,-4.21796379818607,
-0.978688629102168));
#24452=CARTESIAN_POINT('Ctrl Pts',(-4.03083015278197,-1.47755496866388,
-4.07011904373294));
#24453=CARTESIAN_POINT('Ctrl Pts',(-3.91211194281994,2.60783474599474,-3.4566231267461));
#24454=CARTESIAN_POINT('Ctrl Pts',(-3.7933937328579,4.31937746783157,0.303352496851359));
#24455=CARTESIAN_POINT('Ctrl Pts',(-3.67467552289586,2.09909754034784,3.78719321068975));
#24456=CARTESIAN_POINT('Ctrl Pts',(-3.55595731293382,-2.03193881010417,
3.82364600216115));
#24457=CARTESIAN_POINT('Ctrl Pts',(-3.43723910297178,-4.31335160999734,
0.37952828469648));
#24458=CARTESIAN_POINT('Ctrl Pts',(-3.31852089300974,-2.66842714781423,
-3.41006454529105));
#24459=CARTESIAN_POINT('Ctrl Pts',(-3.1998026830477,1.40550049395635,-4.09556005714099));
#24460=CARTESIAN_POINT('Ctrl Pts',(-3.08108447308566,4.20003582720122,-1.05296857580625));
#24461=CARTESIAN_POINT('Ctrl Pts',(-2.96236626312363,3.17138248001238,2.94811412885089));
#24462=CARTESIAN_POINT('Ctrl Pts',(-2.84364805316159,-0.744101854199846,
4.26560150586757));
#24463=CARTESIAN_POINT('Ctrl Pts',(-2.72492984319955,-3.98224868611863,
1.70021738887191));
#24464=CARTESIAN_POINT('Ctrl Pts',(-2.60621163323751,-3.59545308675336,
-2.41283254010238));
#24465=CARTESIAN_POINT('Ctrl Pts',(-2.48749342327547,0.0641944807088134,
-4.32954071903444));
#24466=CARTESIAN_POINT('Ctrl Pts',(-2.36877521331343,3.66540740119438,-2.30517512369736));
#24467=CARTESIAN_POINT('Ctrl Pts',(-2.25005700335139,3.93009067182376,1.81753434046494));
#24468=CARTESIAN_POINT('Ctrl Pts',(-2.13133879338935,0.617309661597382,
4.28578727303431));
#24469=CARTESIAN_POINT('Ctrl Pts',(-2.01262058342732,-3.25739305709507,
2.85279411092906));
#24470=CARTESIAN_POINT('Ctrl Pts',(-1.89390237346528,-4.16697148635381,
-1.17702693243741));
#24471=CARTESIAN_POINT('Ctrl Pts',(-1.77518416350324,-1.28345889131487,
-4.13542948702271));
#24472=CARTESIAN_POINT('Ctrl Pts',(-1.6564659535412,2.76835457083388,-3.32945291871461));
#24473=CARTESIAN_POINT('Ctrl Pts',(-1.53774774357916,4.3002033754076,0.507242247778535));
#24474=CARTESIAN_POINT('Ctrl Pts',(-1.41902953361712,1.91768346415051,3.88220734880688));
#24475=CARTESIAN_POINT('Ctrl Pts',(-1.30031132365508,-2.21045624775848,
3.72329517290076));
#24476=CARTESIAN_POINT('Ctrl Pts',(-1.18159311369304,-4.32647233932304,
0.175159541202699));
#24477=CARTESIAN_POINT('Ctrl Pts',(-1.062874903731,-2.5042077272796,-3.53241948619297));
#24478=CARTESIAN_POINT('Ctrl Pts',(-0.944156693768965,1.59757520747088,
-4.02452447181977));
#24479=CARTESIAN_POINT('Ctrl Pts',(-0.825438483806927,4.24512496593113,
-0.853204425346146));
#24480=CARTESIAN_POINT('Ctrl Pts',(-0.706720273844886,3.02844252168471,
3.09476649533597));
#24481=CARTESIAN_POINT('Ctrl Pts',(-0.588002063882849,-0.944956205417587,
4.22564806126171));
#24482=CARTESIAN_POINT('Ctrl Pts',(-0.46928385392081,-4.05818468348666,
1.51002676880789));
#24483=CARTESIAN_POINT('Ctrl Pts',(-0.350565643958771,-3.47734807176147,
-2.58013452277567));
#24484=CARTESIAN_POINT('Ctrl Pts',(-0.231847433996732,0.268832436023395,
-4.32166320866675));
#24485=CARTESIAN_POINT('Ctrl Pts',(-0.113129224034693,3.77030143007175,
-2.1292888235749));
#24486=CARTESIAN_POINT('Ctrl Pts',(0.00558898592734564,3.83975833568475,
2.00132448427074));
#24487=CARTESIAN_POINT('Ctrl Pts',(0.124307195889385,0.413978250527581,
4.31018164070752));
#24488=CARTESIAN_POINT('Ctrl Pts',(0.243025405851424,-3.38863599139698,
2.69558711334118));
#24489=CARTESIAN_POINT('Ctrl Pts',(0.361743615813462,-4.10665874866663,
-1.37273365581305));
#24490=CARTESIAN_POINT('Ctrl Pts',(0.480461825775502,-1.08649167419266,
-4.19148894901468));
#24491=CARTESIAN_POINT('Ctrl Pts',(0.59918003573754,2.92268188397315,-3.19483557838227));
#24492=CARTESIAN_POINT('Ctrl Pts',(0.717898245699579,4.27141045054158,0.709997556901627));
#24493=CARTESIAN_POINT('Ctrl Pts',(0.836616455661619,1.73197978824728,3.96853748639282));
#24494=CARTESIAN_POINT('Ctrl Pts',(0.955334665623657,-2.38402921411817,
3.61461595111198));
#24495=CARTESIAN_POINT('Ctrl Pts',(1.0740528755857,-4.32991542025907,-0.0296010338436595));
#24496=CARTESIAN_POINT('Ctrl Pts',(1.19277108554774,-2.33438677142145,-3.64687293022593));
#24497=CARTESIAN_POINT('Ctrl Pts',(1.31148929550977,1.78607638655161,-3.94448664710694));
#24498=CARTESIAN_POINT('Ctrl Pts',(1.43020750547181,4.28071840974142,-0.651531783033579));
#24499=CARTESIAN_POINT('Ctrl Pts',(1.54892571543385,2.87872839915225,3.23449633972838));
#24500=CARTESIAN_POINT('Ctrl Pts',(1.66764392539589,-1.14369683351533,4.17624248826731));
#24501=CARTESIAN_POINT('Ctrl Pts',(1.78636213535792,-4.12504314161134,1.31645844888754));
#24502=CARTESIAN_POINT('Ctrl Pts',(1.90508034531997,-3.35146476002329,-2.74166513821877));
#24503=CARTESIAN_POINT('Ctrl Pts',(2.023798555282,0.472869054173783,-4.30411879778042));
#24504=CARTESIAN_POINT('Ctrl Pts',(2.14251676524405,3.86676187041052,-1.94863962941881));
#24505=CARTESIAN_POINT('Ctrl Pts',(2.26123497520608,3.7408370464706,2.18063797076803));
#24506=CARTESIAN_POINT('Ctrl Pts',(2.37995318516813,0.2097208333346,4.32493479024452));
#24507=CARTESIAN_POINT('Ctrl Pts',(2.49867139513016,-3.51229906444054,2.53235049898945));
#24508=CARTESIAN_POINT('Ctrl Pts',(2.6173896050922,-4.03716004244981,-1.56536978361307));
#24509=CARTESIAN_POINT('Ctrl Pts',(2.73610781505424,-0.88709414110546,-4.23817269027803));
#24510=CARTESIAN_POINT('Ctrl Pts',(2.85482602501628,3.07047160403682,-3.05307187871585));
#24511=CARTESIAN_POINT('Ctrl Pts',(2.97354423497831,4.23306303274856,0.911164709906788));
#24512=CARTESIAN_POINT('Ctrl Pts',(3.09226244494036,1.542401938034,4.04599061162419));
#24513=CARTESIAN_POINT('Ctrl Pts',(3.2109806549024,-2.55226947117104,3.49785138539797));
#24514=CARTESIAN_POINT('Ctrl Pts',(3.32969886486443,-4.32367314158497,-0.234295395897341));
#24515=CARTESIAN_POINT('Ctrl Pts',(3.44841707482648,-2.15934414882022,-3.75316887639737));
#24516=CARTESIAN_POINT('Ctrl Pts',(3.56713528478851,1.97058238549235,-3.8556256080939));
#24517=CARTESIAN_POINT('Ctrl Pts',(3.68585349475056,4.30673654014168,-0.448401763612337));
#24518=CARTESIAN_POINT('Ctrl Pts',(3.80457170471259,2.7225750007773,3.36699110972162));
#24519=CARTESIAN_POINT('Ctrl Pts',(3.92328991467463,-1.33987918644085,4.11749529854554));
#24520=CARTESIAN_POINT('Ctrl Pts',(4.04200812463667,-4.18267450812892,1.11994541244234));
#24521=CARTESIAN_POINT('Ctrl Pts',(4.16072633459871,-3.21808473339097,-2.89706306740433));
#24522=CARTESIAN_POINT('Ctrl Pts',(4.27944454456075,0.675847936457875,-4.27694673038929));
#24523=CARTESIAN_POINT('Ctrl Pts',(4.39816275452279,3.95457295490588,-1.76363162597209));
#24524=CARTESIAN_POINT('Ctrl Pts',(4.51688096448482,3.6335480760153,2.35507370311157));
#24525=CARTESIAN_POINT('Ctrl Pts',(4.63559917444687,0.00499430266219868,
4.33001372108024));
#24526=CARTESIAN_POINT('Ctrl Pts',(4.7543173844089,-3.62810566081065,2.36344940326542));
#24527=CARTESIAN_POINT('Ctrl Pts',(4.87303559437094,-3.9586308256988,-1.75450441824159));
#24528=CARTESIAN_POINT('Ctrl Pts',(4.99175380433298,-0.685712313885341,
-4.27537628640897));
#24529=CARTESIAN_POINT('Ctrl Pts',(5.11047201429502,3.21139314798817,-2.90447892346575));
#24530=CARTESIAN_POINT('Ctrl Pts',(5.22919022425705,4.18524689934679,1.11029372659223));
#24531=CARTESIAN_POINT('Ctrl Pts',(5.3479084342191,1.34937397021258,4.11439347368658));
#24532=CARTESIAN_POINT('Ctrl Pts',(5.46662664418113,-2.7148006911525,3.37326266026232));
#24533=CARTESIAN_POINT('Ctrl Pts',(5.58534485414318,-4.30775946632497,-0.438465674927635));
#24534=CARTESIAN_POINT('Ctrl Pts',(5.7040630641052,-1.97947140309336,-3.85106955690723));
#24535=CARTESIAN_POINT('Ctrl Pts',(5.82278127406726,2.1506804925478,-3.75814012335574));
#24536=CARTESIAN_POINT('Ctrl Pts',(5.94149948402928,4.32312115854718,-0.244268737917595));
#24537=CARTESIAN_POINT('Ctrl Pts',(6.06021769399133,2.56033161786722,3.49195443474735));
#24538=CARTESIAN_POINT('Ctrl Pts',(6.17893590395336,-1.53306443422802,4.04953790058903));
#24539=CARTESIAN_POINT('Ctrl Pts',(6.2976541139154,-4.23094987047288,0.920927229126973));
#24540=CARTESIAN_POINT('Ctrl Pts',(6.41637232387744,-3.07750634261675,-3.04598070889424));
#24541=CARTESIAN_POINT('Ctrl Pts',(6.53509053383949,0.87731505011114,-4.24020778625891));
#24542=CARTESIAN_POINT('Ctrl Pts',(6.65380874380152,4.03353826357076,-1.57467864788741));
#24543=CARTESIAN_POINT('Ctrl Pts',(6.77252695376357,3.51813141336254,2.52424149520478));
#24544=CARTESIAN_POINT('Ctrl Pts',(6.89124516372559,-0.199743399502607,
4.32540707242189));
#24545=CARTESIAN_POINT('Ctrl Pts',(7.00996337368766,-3.73579673883507,2.18926163212884));
#24546=CARTESIAN_POINT('Ctrl Pts',(7.12868158364966,-3.87124675627995,-1.93971449440218));
#24547=CARTESIAN_POINT('Ctrl Pts',(7.24739979361173,-0.482796652928421,
-4.30301651864399));
#24548=CARTESIAN_POINT('Ctrl Pts',(7.36611800357374,3.34513129585232,-2.74938909238243));
#24549=CARTESIAN_POINT('Ctrl Pts',(7.4848362135358,4.12806900772511,1.30693918575489));
#24550=CARTESIAN_POINT('Ctrl Pts',(7.60355442349783,1.15332765887133,4.17359306582282));
#24551=CARTESIAN_POINT('Ctrl Pts',(7.72227263345988,-2.87125931654226,3.24112846165826));
#24552=CARTESIAN_POINT('Ctrl Pts',(7.8409908434219,-4.28220999094055,-0.641655173197523));
#24553=CARTESIAN_POINT('Ctrl Pts',(7.95970905338396,-1.79517088210629,-3.94035598288275));
#24554=CARTESIAN_POINT('Ctrl Pts',(8.07842726334599,2.32596785575382,-3.65224825303564));
#24555=CARTESIAN_POINT('Ctrl Pts',(8.19714547330803,4.32983561506851,-0.039589320356336));
#24556=CARTESIAN_POINT('Ctrl Pts',(8.31586368327006,2.39236116409469,3.60910679092953));
#24557=CARTESIAN_POINT('Ctrl Pts',(8.43458189323211,-1.72282045097718,3.97252230471988));
#24558=CARTESIAN_POINT('Ctrl Pts',(8.55330010319414,-4.26976124402944,0.719849072227066));
#24559=CARTESIAN_POINT('Ctrl Pts',(8.67201831315618,-2.93004404009421,-3.18808495666448));
#24560=CARTESIAN_POINT('Ctrl Pts',(8.79073652311822,1.07681974396469,-4.19398414479716));
#24561=CARTESIAN_POINT('Ctrl Pts',(8.90945473308027,4.10348116306779,-1.38220335412341));
#24562=CARTESIAN_POINT('Ctrl Pts',(9.0281729430423,3.39484522796237,2.68776294452898));
#24563=CARTESIAN_POINT('Ctrl Pts',(9.14689115300434,-0.40403430618387,4.3111251486391));
#24564=CARTESIAN_POINT('Ctrl Pts',(9.26560936296638,-3.83513141001683,2.01017681702494));
#24565=CARTESIAN_POINT('Ctrl Pts',(9.38432757292842,-3.77520329901292,-2.12058572543627));
#24566=CARTESIAN_POINT('Ctrl Pts',(9.50304578289045,-0.278801049582681,
-4.32103156000434));
#24567=CARTESIAN_POINT('Ctrl Pts',(9.62176399285249,3.47138689581455,-2.58814929773555));
#24568=CARTESIAN_POINT('Ctrl Pts',(9.74048220281454,4.06165725609586,1.50066122153069));
#24569=CARTESIAN_POINT('Ctrl Pts',(9.85920041277656,0.954701529672213,4.22345696758516));
#24570=CARTESIAN_POINT('Ctrl Pts',(9.97791862273862,-3.02129537328685,3.10174435361097));
#24571=CARTESIAN_POINT('Ctrl Pts',(10.0966368327006,-4.24708186570667,-0.843409386826764));
#24572=CARTESIAN_POINT('Ctrl Pts',(10.2153550426627,-1.60685483798142,-4.02082843422318));
#24573=CARTESIAN_POINT('Ctrl Pts',(10.3340732526247,2.49605238404554,-3.53818686107777));
#24574=CARTESIAN_POINT('Ctrl Pts',(10.4527914625868,4.32686489049173,0.165178652469378));
#24575=CARTESIAN_POINT('Ctrl Pts',(10.5715096725488,2.21903936371554,3.71818612633653));
#24576=CARTESIAN_POINT('Ctrl Pts',(10.6902278825108,-1.9087227814551,3.88662078306603));
#24577=CARTESIAN_POINT('Ctrl Pts',(10.8089460924729,-4.29902181368216,0.517160722873837));
#24578=CARTESIAN_POINT('Ctrl Pts',(10.9276643024349,-2.77602767647701,-3.32305794521066));
#24579=CARTESIAN_POINT('Ctrl Pts',(11.046382512397,1.27391575648429,-4.13837920123483));
#24580=CARTESIAN_POINT('Ctrl Pts',(11.165100722359,4.16424520180891,-1.18663628251469));
#24581=CARTESIAN_POINT('Ctrl Pts',(11.2838189323211,3.26396529218985,2.84527227856014));
#24582=CARTESIAN_POINT('Ctrl Pts',(11.4025371422831,-0.607421449827014,
4.28719989623697));
#24583=CARTESIAN_POINT('Ctrl Pts',(11.5212553522451,-3.9258874778497,1.82659554329586));
#24584=CARTESIAN_POINT('Ctrl Pts',(11.6399735622072,-3.6707152884748,-2.29671352993819));
#24585=CARTESIAN_POINT('Ctrl Pts',(11.7586917721692,-0.0741818108068467,
-4.32938111374782));
#24586=CARTESIAN_POINT('Ctrl Pts',(11.8774099821312,3.5898775332715,-2.42112020803049));
#24587=CARTESIAN_POINT('Ctrl Pts',(11.9961281920933,3.98616019760731,1.69102650674882));
#24588=CARTESIAN_POINT('Ctrl Pts',(12.1148464020553,0.753939878553332,4.26387364210179));
#24589=CARTESIAN_POINT('Ctrl Pts',(12.2335646120174,-3.16457325291087,2.95542211506595));
#24590=CARTESIAN_POINT('Ctrl Pts',(12.3522828219794,-4.20245366825836,-1.04327701860583));
#24591=CARTESIAN_POINT('Ctrl Pts',(12.4710010319414,-1.41494450232315,-4.09230691364976));
#24592=CARTESIAN_POINT('Ctrl Pts',(12.5897192419035,2.66055361930321,-3.41621107150242));
#24593=CARTESIAN_POINT('Ctrl Pts',(12.7084374518655,4.31421563938737,0.369577119444437));
#24594=CARTESIAN_POINT('Ctrl Pts',(12.8271556618275,2.04075389303788,3.81894849741406));
#24595=CARTESIAN_POINT('Ctrl Pts',(12.9458738717896,-2.09035555612641,3.79202538862284));
#24596=CARTESIAN_POINT('Ctrl Pts',(13.0645920817516,-4.31866619344675,0.31331574575378));
#24597=CARTESIAN_POINT('Ctrl Pts',(13.1833102917137,-2.61580163839163,-3.45059810632319));
#24598=CARTESIAN_POINT('Ctrl Pts',(13.3020285016757,1.46816197728233,-4.07351667776667));
#24599=CARTESIAN_POINT('Ctrl Pts',(13.4207467116377,4.2156949100936,-0.98841613733941));
#24600=CARTESIAN_POINT('Ctrl Pts',(13.5394649215998,3.12578350831168,2.9964195514225));
#24601=CARTESIAN_POINT('Ctrl Pts',(13.6581831315618,-0.809448256157549,
4.25368030890243));
#24602=CARTESIAN_POINT('Ctrl Pts',(13.7769013415239,-4.00786503162771,1.63893705711967));
#24603=CARTESIAN_POINT('Ctrl Pts',(13.8956195514859,-3.55801055883195,-2.46772029829628));
#24604=CARTESIAN_POINT('Ctrl Pts',(14.0143377614479,0.130592160376269,-4.32801538634333));
#24605=CARTESIAN_POINT('Ctrl Pts',(14.13305597141,3.70035946541365,-2.248734621409));
#24606=CARTESIAN_POINT('Ctrl Pts',(14.251774181372,3.90170619311096,1.87772177480629));
#24607=CARTESIAN_POINT('Ctrl Pts',(14.370492391334,0.551568832657898,4.29453861879547));
#24608=CARTESIAN_POINT('Ctrl Pts',(14.4892106012961,-3.30091902310761,2.80289624285414));
#24609=CARTESIAN_POINT('Ctrl Pts',(14.6079288112581,-4.14814637637521,-1.24158609289592));
#24610=CARTESIAN_POINT('Ctrl Pts',(14.7266470212202,-1.22040048226755,-4.15315164045192));
#24611=CARTESIAN_POINT('Ctrl Pts',(14.8453652311822,2.82012275334993,-3.28945782906785));
#24612=CARTESIAN_POINT('Ctrl Pts',(14.9640834411443,4.2899026027311,0.579018994044959));
#24613=CARTESIAN_POINT('Ctrl Pts',(15.0432289144523,2.67164257659961,2.79078709004819));
#24614=CARTESIAN_POINT('Ctrl Pts',(15.0828016511063,1.57349100305379,3.31243678044123));
#24615=CARTESIAN_POINT('Ctrl Pts',(-5.72880165110628,-1.62708316297631,
3.44574313044905));
#24616=CARTESIAN_POINT('Ctrl Pts',(-5.68922891445227,-2.76942896202072,
2.90632636444082));
#24617=CARTESIAN_POINT('Ctrl Pts',(-5.61008344114424,-4.45627362126654,
0.611944924532856));
#24618=CARTESIAN_POINT('Ctrl Pts',(-5.4913652311822,-2.93829014436098,-3.41133389386395));
#24619=CARTESIAN_POINT('Ctrl Pts',(-5.37264702122016,1.2581696175504,-4.31848822474448));
#24620=CARTESIAN_POINT('Ctrl Pts',(-5.25392881125812,4.3073857395227,-1.30008227089652));
#24621=CARTESIAN_POINT('Ctrl Pts',(-5.13521060129609,3.43672190219105,2.90459256543017));
#24622=CARTESIAN_POINT('Ctrl Pts',(-5.01649239133405,-0.562844035369692,
4.46380099883135));
#24623=CARTESIAN_POINT('Ctrl Pts',(-4.89777418137201,-4.04978353559191,
1.96050365358111));
#24624=CARTESIAN_POINT('Ctrl Pts',(-4.77905597140997,-3.85045432892764,
-2.32780267938976));
#24625=CARTESIAN_POINT('Ctrl Pts',(-4.66033776144793,-0.146073475978136,
-4.49695172419703));
#24626=CARTESIAN_POINT('Ctrl Pts',(-4.54161955148589,3.69123324660085,-2.57275053391999));
#24627=CARTESIAN_POINT('Ctrl Pts',(-4.42290134152385,4.16852335497868,1.69342154884104));
#24628=CARTESIAN_POINT('Ctrl Pts',(-4.30418313156181,0.851298420661415,
4.41808248628593));
#24629=CARTESIAN_POINT('Ctrl Pts',(-4.18546492159977,-3.24083640963565,
3.12108878930159));
#24630=CARTESIAN_POINT('Ctrl Pts',(-4.06674671163774,-4.3829212061913,-1.01696348095613));
#24631=CARTESIAN_POINT('Ctrl Pts',(-3.9480285016757,-1.53533963668801,-4.22929449422298));
#24632=CARTESIAN_POINT('Ctrl Pts',(-3.82931029171366,2.70982273849253,-3.59180579277186));
#24633=CARTESIAN_POINT('Ctrl Pts',(-3.71059208175162,4.48830099239954,0.31521609833938));
#24634=CARTESIAN_POINT('Ctrl Pts',(-3.59187387178958,2.18118968384959,3.93530391185771));
#24635=CARTESIAN_POINT('Ctrl Pts',(-3.47315566182754,-2.11140448960673,
3.97318231015822));
#24636=CARTESIAN_POINT('Ctrl Pts',(-3.3544374518655,-4.4820394734888,0.394370992008255));
#24637=CARTESIAN_POINT('Ctrl Pts',(-3.23571924190347,-2.77278480634688,
-3.5434263841868));
#24638=CARTESIAN_POINT('Ctrl Pts',(-3.11700103194142,1.46046723372137,-4.25573046250252));
#24639=CARTESIAN_POINT('Ctrl Pts',(-2.99828282197939,4.3642921026776,-1.0941483903534));
#24640=CARTESIAN_POINT('Ctrl Pts',(-2.87956461201734,3.2954098682799,3.06340987069866));
#24641=CARTESIAN_POINT('Ctrl Pts',(-2.76084640205531,-0.773202415284208,
4.43242194379871));
#24642=CARTESIAN_POINT('Ctrl Pts',(-2.64212819209327,-4.13798767600206,
1.76671000638425));
#24643=CARTESIAN_POINT('Ctrl Pts',(-2.52340998213123,-3.73606515697793,
-2.50719432716589));
#24644=CARTESIAN_POINT('Ctrl Pts',(-2.40469177216919,0.066705017937841,
-4.49886171111413));
#24645=CARTESIAN_POINT('Ctrl Pts',(-2.28597356220715,3.80875526597318,-2.3953266118554));
#24646=CARTESIAN_POINT('Ctrl Pts',(-2.16725535224511,4.08378985025871,1.88861502491571));
#24647=CARTESIAN_POINT('Ctrl Pts',(-2.04853714228307,0.641451595143002,
4.45339714207245));
#24648=CARTESIAN_POINT('Ctrl Pts',(-1.92981893232104,-3.38478417310792,
2.96436204859457));
#24649=CARTESIAN_POINT('Ctrl Pts',(-1.811100722359,-4.32993467155617,-1.22305845883667));
#24650=CARTESIAN_POINT('Ctrl Pts',(-1.69238251239696,-1.33365279105472,
-4.29715911814497));
#24651=CARTESIAN_POINT('Ctrl Pts',(-1.57366430243492,2.8766202213453,-3.45966217365956));
#24652=CARTESIAN_POINT('Ctrl Pts',(-1.45494609247288,4.46837703375138,0.527079631508651));
#24653=CARTESIAN_POINT('Ctrl Pts',(-1.33622788251084,1.99268081091691,4.03403389171687));
#24654=CARTESIAN_POINT('Ctrl Pts',(-1.2175096725488,-2.29690344137737,3.86890693021935));
#24655=CARTESIAN_POINT('Ctrl Pts',(-1.09879146258676,-4.49567333227797,
0.182009733685751));
#24656=CARTESIAN_POINT('Ctrl Pts',(-0.980073252624724,-2.60214304288765,
-3.67056641924161));
#24657=CARTESIAN_POINT('Ctrl Pts',(-0.861355042662687,1.66005366341003,
-4.18191679595742));
#24658=CARTESIAN_POINT('Ctrl Pts',(-0.742636832700647,4.4111446011256,-0.886571802886027));
#24659=CARTESIAN_POINT('Ctrl Pts',(-0.623918622738608,3.1468797706921,3.2157975624285));
#24660=CARTESIAN_POINT('Ctrl Pts',(-0.50520041277657,-0.981911839411234,
4.3909059877588));
#24661=CARTESIAN_POINT('Ctrl Pts',(-0.38648220281453,-4.21689340139514,
1.56908135384443));
#24662=CARTESIAN_POINT('Ctrl Pts',(-0.267763992852492,-3.61334125522512,
-2.68103920653919));
#24663=CARTESIAN_POINT('Ctrl Pts',(-0.149045782890452,0.279346016498718,
-4.49067612468082));
#24664=CARTESIAN_POINT('Ctrl Pts',(-0.0303275729284138,3.91775152235812,
-2.21256169694153));
#24665=CARTESIAN_POINT('Ctrl Pts',(0.0883906370336246,3.98992476970996,
2.07959288942982));
#24666=CARTESIAN_POINT('Ctrl Pts',(0.207108846995664,0.430168237555651,
4.47874553207819));
#24667=CARTESIAN_POINT('Ctrl Pts',(0.325827056957703,-3.52115979590533,
2.80100695204636));
#24668=CARTESIAN_POINT('Ctrl Pts',(0.444545266919741,-4.26726320502384,
-1.42641894013007));
#24669=CARTESIAN_POINT('Ctrl Pts',(0.563263476881781,-1.12898252024285,
-4.35541097058569));
#24670=CARTESIAN_POINT('Ctrl Pts',(0.681981686843819,3.03698301387176,-3.31978017753683));
#24671=CARTESIAN_POINT('Ctrl Pts',(0.800699896805858,4.43845806644354,0.737764356779564));
#24672=CARTESIAN_POINT('Ctrl Pts',(0.919418106767898,1.79971457931152,4.12374025451722));
#24673=CARTESIAN_POINT('Ctrl Pts',(1.03813631672994,-2.47726455196977,3.75597744845015));
#24674=CARTESIAN_POINT('Ctrl Pts',(1.15685452669197,-4.49925106626794,-0.0307586800565765));
#24675=CARTESIAN_POINT('Ctrl Pts',(1.27557273665401,-2.42568067756187,-3.78949594329049));
#24676=CARTESIAN_POINT('Ctrl Pts',(1.39429094661605,1.85592680379598,-4.09874882771119));
#24677=CARTESIAN_POINT('Ctrl Pts',(1.51300915657809,4.44813004413594,-0.677012085687766));
#24678=CARTESIAN_POINT('Ctrl Pts',(1.63172736654013,2.9913105828304,3.36099200397128));
#24679=CARTESIAN_POINT('Ctrl Pts',(1.75044557650217,-1.18842487629314,4.33956824662543));
#24680=CARTESIAN_POINT('Ctrl Pts',(1.86916378646421,-4.2863665803859,1.36794290533745));
#24681=CARTESIAN_POINT('Ctrl Pts',(1.98788199642625,-3.48253486073682,-2.84888701030155));
#24682=CARTESIAN_POINT('Ctrl Pts',(2.10660020638828,0.491362160619126,-4.47244558165035));
#24683=CARTESIAN_POINT('Ctrl Pts',(2.22531841635033,4.01798436686502,-2.02484761928903));
#24684=CARTESIAN_POINT('Ctrl Pts',(2.34403662631236,3.88713483670319,2.26591902216312));
#24685=CARTESIAN_POINT('Ctrl Pts',(2.46275483627441,0.217922659316698,4.49407565226358));
#24686=CARTESIAN_POINT('Ctrl Pts',(2.58147304623644,-3.64965912193048,2.63138643065241));
#24687=CARTESIAN_POINT('Ctrl Pts',(2.70019125619848,-4.19504652231746,-1.62658874006443));
#24688=CARTESIAN_POINT('Ctrl Pts',(2.81890946616052,-0.921786887931848,
-4.40392043376685));
#24689=CARTESIAN_POINT('Ctrl Pts',(2.93762767612256,3.19055253914903,-3.17247234009088));
#24690=CARTESIAN_POINT('Ctrl Pts',(3.0563458860846,4.39861094620036,0.946798815841214));
#24691=CARTESIAN_POINT('Ctrl Pts',(3.17506409604663,1.60272266101169,4.20422244007044));
#24692=CARTESIAN_POINT('Ctrl Pts',(3.29378230600868,-2.65208440004178,3.63464641867228));
#24693=CARTESIAN_POINT('Ctrl Pts',(3.41250051597071,-4.49276466266545,-0.243458291328418));
#24694=CARTESIAN_POINT('Ctrl Pts',(3.53121872593276,-2.24379243496572,-3.89994894357639));
#24695=CARTESIAN_POINT('Ctrl Pts',(3.64993693589478,2.04764851932484,-4.00641258422282));
#24696=CARTESIAN_POINT('Ctrl Pts',(3.76865514585684,4.47516569947413,-0.465937995834673));
#24697=CARTESIAN_POINT('Ctrl Pts',(3.88737335581886,2.8290502899728,3.49866841963007));
#24698=CARTESIAN_POINT('Ctrl Pts',(4.00609156578091,-1.39227958820118,4.27852355398336));
#24699=CARTESIAN_POINT('Ctrl Pts',(4.12480977574294,-4.34625181187136,1.16374457743831));
#24700=CARTESIAN_POINT('Ctrl Pts',(4.24352798570499,-3.34393856755371,-3.01036228885148));
#24701=CARTESIAN_POINT('Ctrl Pts',(4.36224619566702,0.702279202618052,-4.44421086080332));
#24702=CARTESIAN_POINT('Ctrl Pts',(4.48096440562906,4.10922959389586,-1.83260426670965));
#24703=CARTESIAN_POINT('Ctrl Pts',(4.5996826155911,3.77564997663844,2.44717664005326));
#24704=CARTESIAN_POINT('Ctrl Pts',(4.71840082555314,0.0051896213660362,
4.49935321146743));
#24705=CARTESIAN_POINT('Ctrl Pts',(4.83711903551518,-3.76999471780869,2.45587989962999));
#24706=CARTESIAN_POINT('Ctrl Pts',(4.95583724547722,-4.11344616113095,-1.82312010936994));
#24707=CARTESIAN_POINT('Ctrl Pts',(5.07455545543925,-0.712529359110903,
-4.44257899942333));
#24708=CARTESIAN_POINT('Ctrl Pts',(5.1932736654013,3.33698528559868,-3.0180681664618));
#24709=CARTESIAN_POINT('Ctrl Pts',(5.31199187536333,4.34892480494547,1.15371543052956));
#24710=CARTESIAN_POINT('Ctrl Pts',(5.43071008532538,1.40214569685748,4.27530042201669));
#24711=CARTESIAN_POINT('Ctrl Pts',(5.54942829528741,-2.82097194028839,3.50518523987218));
#24712=CARTESIAN_POINT('Ctrl Pts',(5.66814650524945,-4.47622863056497,-0.455613323578985));
#24713=CARTESIAN_POINT('Ctrl Pts',(5.78686471521149,-2.05688517132322,-4.00167835360398));
#24714=CARTESIAN_POINT('Ctrl Pts',(5.90558292517353,2.23478995779516,-3.90511460756914));
#24715=CARTESIAN_POINT('Ctrl Pts',(6.02430113513557,4.49219109250754,-0.253821673834409));
#24716=CARTESIAN_POINT('Ctrl Pts',(6.1430193450976,2.66046184361709,3.62851884828642));
#24717=CARTESIAN_POINT('Ctrl Pts',(6.26173755505965,-1.59301998327376,4.20790845748841));
#24718=CARTESIAN_POINT('Ctrl Pts',(6.38045576502168,-4.39641514173326,0.956943130625105));
#24719=CARTESIAN_POINT('Ctrl Pts',(6.49917397498372,-3.19786239441975,-3.16510384664836));
#24720=CARTESIAN_POINT('Ctrl Pts',(6.61789218494576,0.911625353279838,-4.4060351188988));
#24721=CARTESIAN_POINT('Ctrl Pts',(6.73661039490781,4.19128310181113,-1.63626165822722));
#24722=CARTESIAN_POINT('Ctrl Pts',(6.85532860486984,3.65571956412372,2.62296029748738));
#24723=CARTESIAN_POINT('Ctrl Pts',(6.97404681483188,-0.207555024975147,
4.49456640459564));
#24724=CARTESIAN_POINT('Ctrl Pts',(7.09276502479392,-3.88189741118738,2.27487994028893));
#24725=CARTESIAN_POINT('Ctrl Pts',(7.21148323475596,-4.0226446490118,-2.01557343738419));
#24726=CARTESIAN_POINT('Ctrl Pts',(7.330201444718,-0.501678010917997,-4.47130019424702));
#24727=CARTESIAN_POINT('Ctrl Pts',(7.44891965468003,3.47595370552743,-2.85691303520817));
#24728=CARTESIAN_POINT('Ctrl Pts',(7.56763786464208,4.28951078298972,1.35805135997396));
#24729=CARTESIAN_POINT('Ctrl Pts',(7.68635607460411,1.19843234688926,4.33681520976413));
#24730=CARTESIAN_POINT('Ctrl Pts',(7.80507428456615,-2.9835493970715,3.36788349693785));
#24731=CARTESIAN_POINT('Ctrl Pts',(7.92379249452818,-4.44967995854515,-0.666749218397577));
#24732=CARTESIAN_POINT('Ctrl Pts',(8.04251070449024,-1.86537696964218,-4.09445662021724));
#24733=CARTESIAN_POINT('Ctrl Pts',(8.16122891445226,2.41693251238594,-3.79508148585558));
#24734=CARTESIAN_POINT('Ctrl Pts',(8.27994712441432,4.49916814003176,-0.0411375915087343));
#24735=CARTESIAN_POINT('Ctrl Pts',(8.39866533437633,2.48592235037398,3.75025283435974));
#24736=CARTESIAN_POINT('Ctrl Pts',(8.51738354433839,-1.79019703590043,4.12788091232845));
#24737=CARTESIAN_POINT('Ctrl Pts',(8.63610175430042,-4.43674436226274,0.748001148155393));
#24738=CARTESIAN_POINT('Ctrl Pts',(8.75481996426246,-3.04463309142816,-3.31276555045668));
#24739=CARTESIAN_POINT('Ctrl Pts',(8.8735381742245,1.11893233723297,-4.35800374924192));
#24740=CARTESIAN_POINT('Ctrl Pts',(8.99225638418654,4.26396134944328,-1.43625898227515));
#24741=CARTESIAN_POINT('Ctrl Pts',(9.11097459414858,3.52761186517828,2.7928767932663));
#24742=CARTESIAN_POINT('Ctrl Pts',(9.22969280411062,-0.419835402419459,
4.47972593900423));
#24743=CARTESIAN_POINT('Ctrl Pts',(9.34841101407265,-3.98511689282915,2.08879142189926));
#24744=CARTESIAN_POINT('Ctrl Pts',(9.46712922403471,-3.92284509507712,-2.20351823540029));
#24745=CARTESIAN_POINT('Ctrl Pts',(9.58584743399672,-0.289704485621651,
-4.49001977331088));
#24746=CARTESIAN_POINT('Ctrl Pts',(9.70456564395878,3.60714694780058,-2.68936742574997));
#24747=CARTESIAN_POINT('Ctrl Pts',(9.82328385392081,4.22050178042756,1.55934953590272));
#24748=CARTESIAN_POINT('Ctrl Pts',(9.94200206388286,0.992038286763637,4.38862920412596));
#24749=CARTESIAN_POINT('Ctrl Pts',(10.0607202738449,-3.13945310944617,3.22304831290207));
#24750=CARTESIAN_POINT('Ctrl Pts',(10.1794384838069,-4.4131780319313,-0.876393697028316));
#24751=CARTESIAN_POINT('Ctrl Pts',(10.298156693769,-1.66969620452611,-4.17807621260108));
#24752=CARTESIAN_POINT('Ctrl Pts',(10.416874903731,2.59366875801597,-3.67655934637329));
#24753=CARTESIAN_POINT('Ctrl Pts',(10.5355931136931,4.49608123545688,0.171638509327548));
#24754=CARTESIAN_POINT('Ctrl Pts',(10.6543113236551,2.30582222843748,3.86359807751195));
#24755=CARTESIAN_POINT('Ctrl Pts',(10.7730295336171,-1.9833696911239,4.03861992790211));
#24756=CARTESIAN_POINT('Ctrl Pts',(10.8917477435792,-4.46714926315148,0.537386001337347));
#24757=CARTESIAN_POINT('Ctrl Pts',(11.0104659535412,-2.88459340913202,-3.45301710359151));
#24758=CARTESIAN_POINT('Ctrl Pts',(11.1291841635032,1.32373644041171,-4.30022419067547));
#24759=CARTESIAN_POINT('Ctrl Pts',(11.2479023734653,4.3271017666481,-1.23304361429234));
#24760=CARTESIAN_POINT('Ctrl Pts',(11.3666205834273,3.39161343716686,2.95654605012316));
#24761=CARTESIAN_POINT('Ctrl Pts',(11.4853387933893,-0.631176672186531,
4.45486501057192));
#24762=CARTESIAN_POINT('Ctrl Pts',(11.6040570033514,-4.07942227649942,1.8980305960162));
#24763=CARTESIAN_POINT('Ctrl Pts',(11.7227752133134,-3.81427073571983,-2.38653409952016));
#24764=CARTESIAN_POINT('Ctrl Pts',(11.8414934232755,-0.0770829355716051,
-4.49869586393552));
#24765=CARTESIAN_POINT('Ctrl Pts',(11.9602116332375,3.73027155305882,-2.5158061117259));
#24766=CARTESIAN_POINT('Ctrl Pts',(12.0789298431996,4.14205216006884,1.75715968445449));
#24767=CARTESIAN_POINT('Ctrl Pts',(12.1976480531616,0.783425188079069,4.43062650621253));
#24768=CARTESIAN_POINT('Ctrl Pts',(12.3163662631236,-3.28833434385892,3.07100365985594));
#24769=CARTESIAN_POINT('Ctrl Pts',(12.4350844730857,-4.36680450139639,-1.08407781279347));
#24770=CARTESIAN_POINT('Ctrl Pts',(12.5538026830477,-1.47028058123278,-4.2523500940886));
#24771=CARTESIAN_POINT('Ctrl Pts',(12.6725208930097,2.76460335749394,-3.54981329061017));
#24772=CARTESIAN_POINT('Ctrl Pts',(12.7912391029718,4.48293729360237,0.38403065356625));
#24773=CARTESIAN_POINT('Ctrl Pts',(12.9099573129338,2.1205643154784,3.96830109397022));
#24774=CARTESIAN_POINT('Ctrl Pts',(13.0286755228959,-2.17210581545682,3.94032506807154));
#24775=CARTESIAN_POINT('Ctrl Pts',(13.1473937328579,-4.48756190128028,0.325568993002829));
#24776=CARTESIAN_POINT('Ctrl Pts',(13.2661119428199,-2.71810120253451,-3.5855451440222));
#24777=CARTESIAN_POINT('Ctrl Pts',(13.384830152782,1.52557930134958,-4.23282500395937));
#24778=CARTESIAN_POINT('Ctrl Pts',(13.503548362744,4.38056358573491,-1.02707141553694));
#24779=CARTESIAN_POINT('Ctrl Pts',(13.6222665727061,3.2480275981586,3.1136044363927));
#24780=CARTESIAN_POINT('Ctrl Pts',(13.7409847826681,-0.841104404156636,
4.42003452904562));
#24781=CARTESIAN_POINT('Ctrl Pts',(13.8597029926301,-4.16460583332365,1.70303310482458));
#24782=CARTESIAN_POINT('Ctrl Pts',(13.9784212025922,-3.69715831531401,-2.5642286524609));
#24783=CARTESIAN_POINT('Ctrl Pts',(14.0971394125542,0.135699398207657,-4.49727672524931));
#24784=CARTESIAN_POINT('Ctrl Pts',(14.2158576225163,3.84507424612486,-2.33667881727876));
#24785=CARTESIAN_POINT('Ctrl Pts',(14.3345758324783,4.05429530274018,1.95115628770095));
#24786=CARTESIAN_POINT('Ctrl Pts',(14.4532940424403,0.57313975391872,4.46249073811889));
#24787=CARTESIAN_POINT('Ctrl Pts',(14.5720122524024,-3.43001236580562,2.91251275955532));
#24788=CARTESIAN_POINT('Ctrl Pts',(14.6907304623644,-4.31037334346474,-1.29014241853049));
#24789=CARTESIAN_POINT('Ctrl Pts',(14.8094486723265,-1.26812827461363,-4.31557435492763));
#24790=CARTESIAN_POINT('Ctrl Pts',(14.9281668822885,2.93041296965033,-3.41810294391185));
#24791=CARTESIAN_POINT('Ctrl Pts',(15.0468850922505,4.45767341533165,0.60166344454607));
#24792=CARTESIAN_POINT('Ctrl Pts',(15.1260305655585,2.77612598509681,2.89993003832736));
#24793=CARTESIAN_POINT('Ctrl Pts',(15.1656033022126,1.6350275666191,3.44198056308768));
#24794=CARTESIAN_POINT('Ctrl Pts',(-5.646,-1.68832072772979,3.57542852261347));
#24795=CARTESIAN_POINT('Ctrl Pts',(-5.60642726334599,-2.87366031862924,
3.01571004745528));
#24796=CARTESIAN_POINT('Ctrl Pts',(-5.52728179003796,-4.62399175064742,
0.634976333003133));
#24797=CARTESIAN_POINT('Ctrl Pts',(-5.40856358007592,-3.04887682921773,
-3.53972424598284));
#24798=CARTESIAN_POINT('Ctrl Pts',(-5.28984537011389,1.30552260182238,-4.48102060681164));
#24799=CARTESIAN_POINT('Ctrl Pts',(-5.17112716015184,4.4695002639332,-1.34901269686395));
#24800=CARTESIAN_POINT('Ctrl Pts',(-5.0524089501898,3.56606776773373,3.01391099447878));
#24801=CARTESIAN_POINT('Ctrl Pts',(-4.93369074022777,-0.584027462773018,
4.63180243166073));
#24802=CARTESIAN_POINT('Ctrl Pts',(-4.81497253026573,-4.20220283851478,
2.03428996774588));
#24803=CARTESIAN_POINT('Ctrl Pts',(-4.69625432030369,-3.9953715966269,-2.41541280931804));
#24804=CARTESIAN_POINT('Ctrl Pts',(-4.57753611034165,-0.151571156826602,
-4.66620083123102));
#24805=CARTESIAN_POINT('Ctrl Pts',(-4.45881790037962,3.83015800478312,-2.66957962108678));
#24806=CARTESIAN_POINT('Ctrl Pts',(-4.34009969041757,4.32541159811552,1.75715585210948));
#24807=CARTESIAN_POINT('Ctrl Pts',(-4.22138148045554,0.883338234818426,
4.5843632385526));
#24808=CARTESIAN_POINT('Ctrl Pts',(-4.10266327049349,-3.36280984898184,
3.23855535842678));
#24809=CARTESIAN_POINT('Ctrl Pts',(-3.98394506053146,-4.54787861419652,
-1.05523833281009));
#24810=CARTESIAN_POINT('Ctrl Pts',(-3.86522685056942,-1.59312430471214,
-4.38846994471302));
#24811=CARTESIAN_POINT('Ctrl Pts',(-3.74650864060738,2.81181073099031,-3.72698845879762));
#24812=CARTESIAN_POINT('Ctrl Pts',(-3.62779043064534,4.65722451696751,0.327079699827401));
#24813=CARTESIAN_POINT('Ctrl Pts',(-3.5090722206833,2.26328182735134,4.08341461302567));
#24814=CARTESIAN_POINT('Ctrl Pts',(-3.39035401072126,-2.1908701691093,4.12271861815529));
#24815=CARTESIAN_POINT('Ctrl Pts',(-3.27163580075922,-4.65072733698027,
0.409213699320028));
#24816=CARTESIAN_POINT('Ctrl Pts',(-3.15291759079718,-2.87714246487953,
-3.67678822308255));
#24817=CARTESIAN_POINT('Ctrl Pts',(-3.03419938083514,1.51543397348639,-4.41590086786405));
#24818=CARTESIAN_POINT('Ctrl Pts',(-2.91548117087311,4.52854837815398,-1.13532820490054));
#24819=CARTESIAN_POINT('Ctrl Pts',(-2.79676296091107,3.41943725654743,3.17870561254643));
#24820=CARTESIAN_POINT('Ctrl Pts',(-2.67804475094903,-0.802302976368572,
4.59924238172985));
#24821=CARTESIAN_POINT('Ctrl Pts',(-2.55932654098699,-4.2937266658855,1.83320262389659));
#24822=CARTESIAN_POINT('Ctrl Pts',(-2.44060833102495,-3.87667722720249,
-2.6015561142294));
#24823=CARTESIAN_POINT('Ctrl Pts',(-2.32189012106291,0.0692155551668676,
-4.6681827031938));
#24824=CARTESIAN_POINT('Ctrl Pts',(-2.20317191110087,3.95210313075198,-2.48547810001344));
#24825=CARTESIAN_POINT('Ctrl Pts',(-2.08445370113884,4.23748902869366,1.95969570936649));
#24826=CARTESIAN_POINT('Ctrl Pts',(-1.96573549117679,0.665593528688616,
4.62100701111058));
#24827=CARTESIAN_POINT('Ctrl Pts',(-1.84701728121476,-3.51217528912075,
3.07592998626008));
#24828=CARTESIAN_POINT('Ctrl Pts',(-1.72829907125272,-4.49289785675852,
-1.26908998523592));
#24829=CARTESIAN_POINT('Ctrl Pts',(-1.60958086129068,-1.38384669079458,
-4.45888874926723));
#24830=CARTESIAN_POINT('Ctrl Pts',(-1.49086265132864,2.98488587185672,-3.58987142860451));
#24831=CARTESIAN_POINT('Ctrl Pts',(-1.3721444413666,4.63655069209516,0.546917015238768));
#24832=CARTESIAN_POINT('Ctrl Pts',(-1.25342623140456,2.06767815768332,4.18586043462686));
#24833=CARTESIAN_POINT('Ctrl Pts',(-1.13470802144252,-2.38335063499626,
4.01451868753794));
#24834=CARTESIAN_POINT('Ctrl Pts',(-1.01598981148048,-4.66487432523292,
0.188859926168807));
#24835=CARTESIAN_POINT('Ctrl Pts',(-0.897271601518447,-2.70007835849569,
-3.80871335229026));
#24836=CARTESIAN_POINT('Ctrl Pts',(-0.778553391556407,1.72253211934917,
-4.33930912009507));
#24837=CARTESIAN_POINT('Ctrl Pts',(-0.659835181594369,4.57716423632007,
-0.919939180425913));
#24838=CARTESIAN_POINT('Ctrl Pts',(-0.541116971632329,3.26531701969948,
3.33682862952102));
#24839=CARTESIAN_POINT('Ctrl Pts',(-0.422398761670291,-1.01886747340488,
4.5561639142559));
#24840=CARTESIAN_POINT('Ctrl Pts',(-0.303680551708251,-4.37560211930362,
1.62813593888096));
#24841=CARTESIAN_POINT('Ctrl Pts',(-0.184962341746213,-3.74933443868876,
-2.78194389030271));
#24842=CARTESIAN_POINT('Ctrl Pts',(-0.0662441317841735,0.289859596974037,
-4.6596890406949));
#24843=CARTESIAN_POINT('Ctrl Pts',(0.0524740781778654,4.06520161464448,
-2.29583457030816));
#24844=CARTESIAN_POINT('Ctrl Pts',(0.171192288139903,4.14009120373516,2.1578612945889));
#24845=CARTESIAN_POINT('Ctrl Pts',(0.289910498101944,0.446358224583725,
4.64730942344886));
#24846=CARTESIAN_POINT('Ctrl Pts',(0.40862870806398,-3.65368360041369,2.90642679075152));
#24847=CARTESIAN_POINT('Ctrl Pts',(0.527346918026022,-4.42786766138104,
-1.4801042244471));
#24848=CARTESIAN_POINT('Ctrl Pts',(0.646065127988058,-1.17147336629305,
-4.51933299215671));
#24849=CARTESIAN_POINT('Ctrl Pts',(0.764783337950099,3.15128414377037,-3.44472477669139));
#24850=CARTESIAN_POINT('Ctrl Pts',(0.883501547912136,4.60550568234552,0.765531156657499));
#24851=CARTESIAN_POINT('Ctrl Pts',(1.00221975787418,1.86744937037575,4.27894302264161));
#24852=CARTESIAN_POINT('Ctrl Pts',(1.12093796783621,-2.57049988982138,3.89733894578832));
#24853=CARTESIAN_POINT('Ctrl Pts',(1.23965617779826,-4.6685867122768,-0.0319163262694973));
#24854=CARTESIAN_POINT('Ctrl Pts',(1.35837438776029,-2.5169745837023,-3.93211895635505));
#24855=CARTESIAN_POINT('Ctrl Pts',(1.47709259772233,1.92577722104035,-4.25301100831545));
#24856=CARTESIAN_POINT('Ctrl Pts',(1.59581080768437,4.61554167853046,-0.70249238834195));
#24857=CARTESIAN_POINT('Ctrl Pts',(1.71452901764641,3.10389276650854,3.48748766821418));
#24858=CARTESIAN_POINT('Ctrl Pts',(1.83324722760845,-1.23315291907095,4.50289400498357));
#24859=CARTESIAN_POINT('Ctrl Pts',(1.95196543757049,-4.44769001916047,1.41942736178737));
#24860=CARTESIAN_POINT('Ctrl Pts',(2.07068364753253,-3.61360496145035,-2.95610888238434));
#24861=CARTESIAN_POINT('Ctrl Pts',(2.18940185749457,0.509855267064465,-4.64077236552028));
#24862=CARTESIAN_POINT('Ctrl Pts',(2.3081200674566,4.16920686331953,-2.10105560915926));
#24863=CARTESIAN_POINT('Ctrl Pts',(2.42683827741864,4.03343262693579,2.35120007355821));
#24864=CARTESIAN_POINT('Ctrl Pts',(2.54555648738068,0.226124485298797,4.66321651428264));
#24865=CARTESIAN_POINT('Ctrl Pts',(2.66427469734272,-3.78701917942043,2.73042236231537));
#24866=CARTESIAN_POINT('Ctrl Pts',(2.78299290730476,-4.35293300218511,-1.6878076965158));
#24867=CARTESIAN_POINT('Ctrl Pts',(2.9017111172668,-0.956479634758229,-4.56966817725565));
#24868=CARTESIAN_POINT('Ctrl Pts',(3.02042932722884,3.31063347426123,-3.29187280146591));
#24869=CARTESIAN_POINT('Ctrl Pts',(3.13914753719087,4.56415885965217,0.982432921775639));
#24870=CARTESIAN_POINT('Ctrl Pts',(3.25786574715291,1.66304338398937,4.36245426851668));
#24871=CARTESIAN_POINT('Ctrl Pts',(3.37658395711496,-2.75189932891252,3.7714414519466));
#24872=CARTESIAN_POINT('Ctrl Pts',(3.49530216707699,-4.66185618374594,-0.252621186759496));
#24873=CARTESIAN_POINT('Ctrl Pts',(3.61402037703904,-2.32824072111122,-4.04672901075542));
#24874=CARTESIAN_POINT('Ctrl Pts',(3.73273858700106,2.12471465315734,-4.15719956035174));
#24875=CARTESIAN_POINT('Ctrl Pts',(3.85145679696312,4.64359485880658,-0.483474228057011));
#24876=CARTESIAN_POINT('Ctrl Pts',(3.97017500692514,2.93552557916831,3.63034572953853));
#24877=CARTESIAN_POINT('Ctrl Pts',(4.08889321688719,-1.44467998996152,4.43955180942118));
#24878=CARTESIAN_POINT('Ctrl Pts',(4.20761142684922,-4.50982911561381,1.20754374243428));
#24879=CARTESIAN_POINT('Ctrl Pts',(4.32632963681127,-3.46979240171644,-3.12366151029863));
#24880=CARTESIAN_POINT('Ctrl Pts',(4.4450478467733,0.728710468778227,-4.61147499121735));
#24881=CARTESIAN_POINT('Ctrl Pts',(4.56376605673534,4.26388623288585,-1.90157690744722));
#24882=CARTESIAN_POINT('Ctrl Pts',(4.68248426669738,3.91775187726159,2.53927957699493));
#24883=CARTESIAN_POINT('Ctrl Pts',(4.80120247665942,0.00538494006987035,
4.66869270185463));
#24884=CARTESIAN_POINT('Ctrl Pts',(4.91992068662146,-3.91188377480672,2.54831039599456));
#24885=CARTESIAN_POINT('Ctrl Pts',(5.03863889658349,-4.2682614965631,-1.8917358004983));
#24886=CARTESIAN_POINT('Ctrl Pts',(5.15735710654554,-0.739346404336463,
-4.60978171243769));
#24887=CARTESIAN_POINT('Ctrl Pts',(5.27607531650758,3.46257742320919,-3.13165740945785));
#24888=CARTESIAN_POINT('Ctrl Pts',(5.39479352646961,4.51260271054416,1.19713713446688));
#24889=CARTESIAN_POINT('Ctrl Pts',(5.51351173643165,1.45491742350237,4.4362073703468));
#24890=CARTESIAN_POINT('Ctrl Pts',(5.63222994639369,-2.92714318942428,3.63710781948203));
#24891=CARTESIAN_POINT('Ctrl Pts',(5.75094815635573,-4.64469779480496,-0.47276097223033));
#24892=CARTESIAN_POINT('Ctrl Pts',(5.86966636631777,-2.13429893955308,-4.15228715030074));
#24893=CARTESIAN_POINT('Ctrl Pts',(5.98838457627981,2.31889942304252,-4.05208909178254));
#24894=CARTESIAN_POINT('Ctrl Pts',(6.10710278624184,4.6612610264679,-0.263374609751229));
#24895=CARTESIAN_POINT('Ctrl Pts',(6.2258209962039,2.76059206936697,3.76508326182549));
#24896=CARTESIAN_POINT('Ctrl Pts',(6.34453920616592,-1.65297553231951,4.36627901438777));
#24897=CARTESIAN_POINT('Ctrl Pts',(6.46325741612797,-4.56188041299363,0.992959032123235));
#24898=CARTESIAN_POINT('Ctrl Pts',(6.58197562609,-3.31821844622275,-3.28422698440246));
#24899=CARTESIAN_POINT('Ctrl Pts',(6.70069383605205,0.945935656448541,-4.57186245153871));
#24900=CARTESIAN_POINT('Ctrl Pts',(6.81941204601407,4.34902794005149,-1.69784466856703));
#24901=CARTESIAN_POINT('Ctrl Pts',(6.93813025597612,3.7933077148849,2.72167909976998));
#24902=CARTESIAN_POINT('Ctrl Pts',(7.05684846593816,-0.215366650447688,
4.66372573676938));
#24903=CARTESIAN_POINT('Ctrl Pts',(7.1755666759002,-4.02799808353968,2.36049824844903));
#24904=CARTESIAN_POINT('Ctrl Pts',(7.29428488586223,-4.17404254174364,-2.09143238036622));
#24905=CARTESIAN_POINT('Ctrl Pts',(7.41300309582428,-0.520559368907565,
-4.63958386985003));
#24906=CARTESIAN_POINT('Ctrl Pts',(7.53172130578631,3.60677611520251,-2.96443697803392));
#24907=CARTESIAN_POINT('Ctrl Pts',(7.65043951574836,4.45095255825434,1.40916353419305));
#24908=CARTESIAN_POINT('Ctrl Pts',(7.76915772571038,1.24353703490719,4.50003735370544));
#24909=CARTESIAN_POINT('Ctrl Pts',(7.88787593567244,-3.09583947760073,3.49463853221744));
#24910=CARTESIAN_POINT('Ctrl Pts',(8.00659414563446,-4.61714992614977,-0.691843263597633));
#24911=CARTESIAN_POINT('Ctrl Pts',(8.12531235559652,-1.93558305717806,-4.24855725755173));
#24912=CARTESIAN_POINT('Ctrl Pts',(8.24403056555854,2.50789716901805,-3.93791471867551));
#24913=CARTESIAN_POINT('Ctrl Pts',(8.36274877552059,4.66850066499502,-0.0426858626611376));
#24914=CARTESIAN_POINT('Ctrl Pts',(8.48146698548262,2.57948353665327,3.89139887778996));
#24915=CARTESIAN_POINT('Ctrl Pts',(8.60018519544467,-1.85757362082367,4.28323951993702));
#24916=CARTESIAN_POINT('Ctrl Pts',(8.7189034054067,-4.60372748049605,0.776153224083728));
#24917=CARTESIAN_POINT('Ctrl Pts',(8.83762161536874,-3.15922214276211,-3.4374461442489));
#24918=CARTESIAN_POINT('Ctrl Pts',(8.95633982533078,1.16104493050125,-4.52202335368666));
#24919=CARTESIAN_POINT('Ctrl Pts',(9.07505803529283,4.42444153581877,-1.4903146104269));
#24920=CARTESIAN_POINT('Ctrl Pts',(9.19377624525485,3.66037850239417,2.89799064200363));
#24921=CARTESIAN_POINT('Ctrl Pts',(9.3124944552169,-0.435636498655038,4.64832672936936));
#24922=CARTESIAN_POINT('Ctrl Pts',(9.43121266517893,-4.13510237564149,2.16740602677358));
#24923=CARTESIAN_POINT('Ctrl Pts',(9.54993087514098,-4.07048689114132,-2.2864507453643));
#24924=CARTESIAN_POINT('Ctrl Pts',(9.66864908510301,-0.300607921660628,
-4.65900798661742));
#24925=CARTESIAN_POINT('Ctrl Pts',(9.78736729506505,3.74290699978661,-2.79058555376438));
#24926=CARTESIAN_POINT('Ctrl Pts',(9.90608550502709,4.37934630475926,1.61803785027473));
#24927=CARTESIAN_POINT('Ctrl Pts',(10.0248037149891,1.02937504385506,4.55380144066675));
#24928=CARTESIAN_POINT('Ctrl Pts',(10.1435219249512,-3.2576108456055,3.34435227219316));
#24929=CARTESIAN_POINT('Ctrl Pts',(10.2622401349132,-4.57927419815593,-0.909378007229871));
#24930=CARTESIAN_POINT('Ctrl Pts',(10.3809583448752,-1.73253757107079,-4.33532399097899));
#24931=CARTESIAN_POINT('Ctrl Pts',(10.4996765548373,2.69128513198641,-3.8149318316688));
#24932=CARTESIAN_POINT('Ctrl Pts',(10.6183947647993,4.66529758042202,0.178098366185712));
#24933=CARTESIAN_POINT('Ctrl Pts',(10.7371129747614,2.39260509315942,4.00901002868737));
#24934=CARTESIAN_POINT('Ctrl Pts',(10.8558311847234,-2.05801660079268,4.19061907273819));
#24935=CARTESIAN_POINT('Ctrl Pts',(10.9745493946854,-4.63527671262081,0.557611279800856));
#24936=CARTESIAN_POINT('Ctrl Pts',(11.0932676046475,-2.99315914178703,-3.58297626197237));
#24937=CARTESIAN_POINT('Ctrl Pts',(11.2119858146095,1.37355712433912,-4.46206918011612));
#24938=CARTESIAN_POINT('Ctrl Pts',(11.3307040245716,4.48995833148729,-1.27945094606998));
#24939=CARTESIAN_POINT('Ctrl Pts',(11.4494222345336,3.51926158214387,3.06781982168619));
#24940=CARTESIAN_POINT('Ctrl Pts',(11.5681404444956,-0.654931894546049,
4.62253012490687));
#24941=CARTESIAN_POINT('Ctrl Pts',(11.6868586544577,-4.23295707514914,1.96946564873655));
#24942=CARTESIAN_POINT('Ctrl Pts',(11.8055768644197,-3.95782618296486,-2.47635466910213));
#24943=CARTESIAN_POINT('Ctrl Pts',(11.9242950743818,-0.0799840603363634,
-4.66801061412323));
#24944=CARTESIAN_POINT('Ctrl Pts',(12.0430132843438,3.87066557284614,-2.61049201542129));
#24945=CARTESIAN_POINT('Ctrl Pts',(12.1617314943058,4.29794412253036,1.82329286216014));
#24946=CARTESIAN_POINT('Ctrl Pts',(12.2804497042679,0.812910497604809,4.59737937032327));
#24947=CARTESIAN_POINT('Ctrl Pts',(12.3991679142299,-3.41209543480698,3.18658520464592));
#24948=CARTESIAN_POINT('Ctrl Pts',(12.5178861241919,-4.53115533453443,-1.12487860698111));
#24949=CARTESIAN_POINT('Ctrl Pts',(12.636604334154,-1.52561666014242,-4.41239327452744));
#24950=CARTESIAN_POINT('Ctrl Pts',(12.755322544116,2.86865309568467,-3.68341550971791));
#24951=CARTESIAN_POINT('Ctrl Pts',(12.8740407540781,4.65165894781738,0.398484187688063));
#24952=CARTESIAN_POINT('Ctrl Pts',(12.9927589640401,2.20037473791892,4.11765369052636));
#24953=CARTESIAN_POINT('Ctrl Pts',(13.1114771740021,-2.25385607478723,4.08862474752024));
#24954=CARTESIAN_POINT('Ctrl Pts',(13.2301953839642,-4.6564576091138,0.337822240251874));
#24955=CARTESIAN_POINT('Ctrl Pts',(13.3489135939262,-2.82040076667739,-3.72049218172121));
#24956=CARTESIAN_POINT('Ctrl Pts',(13.4676318038883,1.58299662541684,-4.39213333015208));
#24957=CARTESIAN_POINT('Ctrl Pts',(13.5863500138503,4.54543226137621,-1.06572669373447));
#24958=CARTESIAN_POINT('Ctrl Pts',(13.7050682238123,3.37027168800554,3.2307893213629));
#24959=CARTESIAN_POINT('Ctrl Pts',(13.8237864337744,-0.872760552155723,
4.58638874918879));
#24960=CARTESIAN_POINT('Ctrl Pts',(13.9425046437364,-4.32134663501959,1.76712915252949));
#24961=CARTESIAN_POINT('Ctrl Pts',(14.0612228536984,-3.83630607179607,-2.66073700662553));
#24962=CARTESIAN_POINT('Ctrl Pts',(14.1799410636605,0.140806636039052,-4.6665380641553));
#24963=CARTESIAN_POINT('Ctrl Pts',(14.2986592736225,3.98978902683606,-2.42462301314851));
#24964=CARTESIAN_POINT('Ctrl Pts',(14.4173774835846,4.20688441236941,2.0245908005956));
#24965=CARTESIAN_POINT('Ctrl Pts',(14.5360956935466,0.594710675179534,4.63044285744233));
#24966=CARTESIAN_POINT('Ctrl Pts',(14.6548139035086,-3.55910570850363,3.02212927625648));
#24967=CARTESIAN_POINT('Ctrl Pts',(14.7735321134707,-4.47260031055426,-1.33869874416505));
#24968=CARTESIAN_POINT('Ctrl Pts',(14.8922503234327,-1.31585606695972,-4.47799706940333));
#24969=CARTESIAN_POINT('Ctrl Pts',(15.0109685333948,3.04070318595074,-3.54674805875586));
#24970=CARTESIAN_POINT('Ctrl Pts',(15.1296867433568,4.62544422793221,0.624307895047183));
#24971=CARTESIAN_POINT('Ctrl Pts',(15.2088322166648,2.880609393594,3.00907298660654));
#24972=CARTESIAN_POINT('Ctrl Pts',(15.2484049533188,1.69656413018441,3.57152434573413));
#24973=CARTESIAN_POINT('Ctrl Pts',(14.7388401553692,-3.95165589089271,-0.00363582964324092));
#24974=CARTESIAN_POINT('Ctrl Pts',(14.7504041414031,-3.95480700531195,-0.38716052775308));
#24975=CARTESIAN_POINT('Ctrl Pts',(14.7619681274369,-3.90348129134194,-0.769828015324074));
#24976=CARTESIAN_POINT('Ctrl Pts',(14.7735321134707,-3.79422716961339,-1.13511046163454));
#24977=CARTESIAN_POINT('Ctrl Pts',(14.8131048501247,-3.42035222935605,-2.38513151924453));
#24978=CARTESIAN_POINT('Ctrl Pts',(14.8526775867787,-2.36810414815783,-3.43156429432397));
#24979=CARTESIAN_POINT('Ctrl Pts',(14.8922503234327,-1.11588689874029,-3.79957251342241));
#24980=CARTESIAN_POINT('Ctrl Pts',(14.9281668822885,0.0206363326986077,
-4.13357996345584));
#24981=CARTESIAN_POINT('Ctrl Pts',(14.9640834411442,1.32188486567401,-3.90873281330822));
#24982=CARTESIAN_POINT('Ctrl Pts',(15.,2.29296287427331,-3.22854765929654));
#24983=CARTESIAN_POINT('',(-5.646,-2.04569608541847,-2.86913603522098));
#24984=CARTESIAN_POINT('Ctrl Pts',(-5.646,-2.05008858489997,-2.8725153718199));
#24985=CARTESIAN_POINT('Ctrl Pts',(-5.646,-2.14207707493584,-2.81555118308838));
#24986=CARTESIAN_POINT('Ctrl Pts',(-5.646,-2.23107770091101,-2.7542618031163));
#24987=CARTESIAN_POINT('Ctrl Pts',(-5.646,-2.31673031453871,-2.68871061623223));
#24988=CARTESIAN_POINT('Ctrl Pts',(-5.646,-2.4049668623091,-2.6211819070904));
#24989=CARTESIAN_POINT('Ctrl Pts',(-5.646,-2.48965143582115,-2.54913073294227));
#24990=CARTESIAN_POINT('Ctrl Pts',(-5.646,-2.57069342680521,-2.47296330102159));
#24991=CARTESIAN_POINT('Ctrl Pts',(-5.646,-2.62057798544578,-2.42607922675328));
#24992=CARTESIAN_POINT('Ctrl Pts',(-5.646,-2.66908188885062,-2.37763460603863));
#24993=CARTESIAN_POINT('Ctrl Pts',(-5.646,-2.71617833586228,-2.32771640428473));
#24994=CARTESIAN_POINT('Ctrl Pts',(-5.646,-2.73123404318985,-2.31175864348508));
#24995=CARTESIAN_POINT('Ctrl Pts',(-5.646,-2.74614588109029,-2.29565025093888));
#24996=CARTESIAN_POINT('Ctrl Pts',(-5.646,-2.76091287095153,-2.27939395874847));
#24997=CARTESIAN_POINT('Ctrl Pts',(-5.646,-2.77497190065622,-2.26391702696071));
#24998=CARTESIAN_POINT('Ctrl Pts',(-5.646,-2.78889460108938,-2.24831151965524));
#24999=CARTESIAN_POINT('Ctrl Pts',(-5.646,-2.80267583839923,-2.2325853908502));
#25000=CARTESIAN_POINT('Ctrl Pts',(-5.646,-2.87737822131438,-2.14734055619902));
#25001=CARTESIAN_POINT('Ctrl Pts',(-5.646,-2.94796949551254,-2.05850773745867));
#25002=CARTESIAN_POINT('Ctrl Pts',(-5.646,-3.01435939466491,-1.96650898761472));
#25003=CARTESIAN_POINT('Ctrl Pts',(-5.646,-3.07837534811936,-1.87779989537221));
#25004=CARTESIAN_POINT('Ctrl Pts',(-5.646,-3.13848514835476,-1.78614641339449));
#25005=CARTESIAN_POINT('Ctrl Pts',(-5.646,-3.19457903134324,-1.69189377245409));
#25006=CARTESIAN_POINT('Ctrl Pts',(-5.646,-3.2191201051507,-1.65065824204266));
#25007=CARTESIAN_POINT('Ctrl Pts',(-5.646,-3.24289211518763,-1.60892485034322));
#25008=CARTESIAN_POINT('Ctrl Pts',(-5.646,-3.26588393940166,-1.56672099319786));
#25009=CARTESIAN_POINT('Ctrl Pts',(-5.646,-3.27889011824424,-1.54284681476081));
#25010=CARTESIAN_POINT('Ctrl Pts',(-5.646,-3.29164661390766,-1.51882207153166));
#25011=CARTESIAN_POINT('Ctrl Pts',(-5.646,-3.30415123343052,-1.49465161725134));
#25012=CARTESIAN_POINT('Ctrl Pts',(-5.646,-3.31300408836539,-1.47753973911205));
#25013=CARTESIAN_POINT('Ctrl Pts',(-5.646,-3.32172655541921,-1.46036277478602));
#25014=CARTESIAN_POINT('Ctrl Pts',(-5.646,-3.3303159831105,-1.44312718454166));
#25015=CARTESIAN_POINT('Ctrl Pts',(-5.646,-3.38286439723767,-1.33768326366137));
#25016=CARTESIAN_POINT('Ctrl Pts',(-5.646,-3.43046401145348,-1.22999506945072));
#25017=CARTESIAN_POINT('Ctrl Pts',(-5.646,-3.473014032799,-1.12050081343609));
#25018=CARTESIAN_POINT('Ctrl Pts',(-5.646,-3.51603566968294,-1.00979294598551));
#25019=CARTESIAN_POINT('Ctrl Pts',(-5.646,-3.55389562836961,-0.897237988908388));
#25020=CARTESIAN_POINT('Ctrl Pts',(-5.646,-3.5864484949203,-0.783255416256629));
#25021=CARTESIAN_POINT('Ctrl Pts',(-5.646,-3.6186577594367,-0.670475952516229));
#25022=CARTESIAN_POINT('Ctrl Pts',(-5.646,-3.64567169970723,-0.556298001248345));
#25023=CARTESIAN_POINT('Ctrl Pts',(-5.646,-3.66730359446243,-0.441107587639058));
#25024=CARTESIAN_POINT('Ctrl Pts',(-5.646,-3.68198751655827,-0.362915312816758));
#25025=CARTESIAN_POINT('Ctrl Pts',(-5.646,-3.69419054645532,-0.284256101620809));
#25026=CARTESIAN_POINT('Ctrl Pts',(-5.646,-3.70384084236009,-0.205248270572724));
#25027=CARTESIAN_POINT('Ctrl Pts',(-5.646,-3.70640721713813,-0.184237131964063));
#25028=CARTESIAN_POINT('Ctrl Pts',(-5.646,-3.70879299259457,-0.163201334056653));
#25029=CARTESIAN_POINT('Ctrl Pts',(-5.646,-3.71099667802055,-0.142143098155404));
#25030=CARTESIAN_POINT('Ctrl Pts',(-5.646,-3.71270249148621,-0.125842485581626));
#25031=CARTESIAN_POINT('Ctrl Pts',(-5.646,-3.71429910512685,-0.109528708261293));
#25032=CARTESIAN_POINT('Ctrl Pts',(-5.646,-3.71578473600114,-0.0932167080416795));
#25033=CARTESIAN_POINT('Ctrl Pts',(-5.646,-3.72667009638022,0.0263028872816144));
#25034=CARTESIAN_POINT('Ctrl Pts',(-5.646,-3.73162164541571,0.145914627178937));
#25035=CARTESIAN_POINT('Ctrl Pts',(-5.646,-3.73049871915079,0.26519666316469));
#25036=CARTESIAN_POINT('Ctrl Pts',(-5.646,-3.72973942409088,0.345852235564089));
#25037=CARTESIAN_POINT('Ctrl Pts',(-5.646,-3.72620187382023,0.426357611138785));
#25038=CARTESIAN_POINT('Ctrl Pts',(-5.646,-3.71982963805668,0.506586333723297));
#25039=CARTESIAN_POINT('Ctrl Pts',(-5.646,-3.71064929233637,0.622170162909031));
#25040=CARTESIAN_POINT('Ctrl Pts',(-5.646,-3.69558794607162,0.7371801151484));
#25041=CARTESIAN_POINT('Ctrl Pts',(-5.646,-3.67492250378245,0.851326378345511));
#25042=CARTESIAN_POINT('Ctrl Pts',(-5.646,-3.65389180309679,0.967490158539211));
#25043=CARTESIAN_POINT('Ctrl Pts',(-5.646,-3.62705693335592,1.08276014959161));
#25044=CARTESIAN_POINT('Ctrl Pts',(-5.646,-3.59465621011333,1.19682455346059));
#25045=CARTESIAN_POINT('Ctrl Pts',(-5.646,-3.58656895937205,1.22529513505337));
#25046=CARTESIAN_POINT('Ctrl Pts',(-5.646,-3.57813470527536,1.25369054778353));
#25047=CARTESIAN_POINT('Ctrl Pts',(-5.646,-3.56935667185545,1.28200580159195));
#25048=CARTESIAN_POINT('Ctrl Pts',(-5.646,-3.5632475546913,1.30171194700898));
#25049=CARTESIAN_POINT('Ctrl Pts',(-5.646,-3.5569709708608,1.32138188327048));
#25050=CARTESIAN_POINT('Ctrl Pts',(-5.646,-3.55053584166857,1.34099072546513));
#25051=CARTESIAN_POINT('Ctrl Pts',(-5.646,-3.51190829019201,1.45869489870602));
#25052=CARTESIAN_POINT('Ctrl Pts',(-5.646,-3.46752131199915,1.57437189095583));
#25053=CARTESIAN_POINT('Ctrl Pts',(-5.646,-3.4177365460153,1.68768626856115));
#25054=CARTESIAN_POINT('Ctrl Pts',(-5.646,-3.36898689227503,1.79864464233047));
#25055=CARTESIAN_POINT('Ctrl Pts',(-5.646,-3.31506092584505,1.90733835387831));
#25056=CARTESIAN_POINT('Ctrl Pts',(-5.646,-3.25624215907454,2.01344625944578));
#25057=CARTESIAN_POINT('Ctrl Pts',(-5.646,-3.19710665592352,2.1201255512527));
#25058=CARTESIAN_POINT('Ctrl Pts',(-5.646,-3.13302512594978,2.22419187938599));
#25059=CARTESIAN_POINT('Ctrl Pts',(-5.646,-3.06423583750868,2.32530137231072));
#25060=CARTESIAN_POINT('Ctrl Pts',(-5.646,-3.02024766893345,2.38995709880711));
#25061=CARTESIAN_POINT('Ctrl Pts',(-5.646,-2.97433345310045,2.45340335435671));
#25062=CARTESIAN_POINT('Ctrl Pts',(-5.646,-2.92654602325611,2.515544268775));
#25063=CARTESIAN_POINT('Ctrl Pts',(-5.646,-2.9070747480676,2.54086395742628));
#25064=CARTESIAN_POINT('Ctrl Pts',(-5.646,-2.88729240115396,2.56596686978521));
#25065=CARTESIAN_POINT('Ctrl Pts',(-5.646,-2.86720223741143,2.59084624023121));
#25066=CARTESIAN_POINT('Ctrl Pts',(-5.646,-2.8548315572927,2.60616591294702));
#25067=CARTESIAN_POINT('Ctrl Pts',(-5.646,-2.84234310750814,2.62140196742225));
#25068=CARTESIAN_POINT('Ctrl Pts',(-5.646,-2.82975126313558,2.63653676106713));
#25069=CARTESIAN_POINT('Ctrl Pts',(-5.646,-2.75009555303069,2.73227910820889));
#25070=CARTESIAN_POINT('Ctrl Pts',(-5.646,-2.66618789926205,2.82411933161441));
#25071=CARTESIAN_POINT('Ctrl Pts',(-5.646,-2.57832047400345,2.91172962772101));
#25072=CARTESIAN_POINT('Ctrl Pts',(-5.646,-2.49061075100628,2.99918268305518));
#25073=CARTESIAN_POINT('Ctrl Pts',(-5.646,-2.39895497729817,3.0824217324784));
#25074=CARTESIAN_POINT('Ctrl Pts',(-5.646,-2.30359796366059,3.16109653178087));
#25075=CARTESIAN_POINT('Ctrl Pts',(-5.646,-2.20819311932976,3.23981079404521));
#25076=CARTESIAN_POINT('Ctrl Pts',(-5.646,-2.10908286731295,3.31395700277454));
#25077=CARTESIAN_POINT('Ctrl Pts',(-5.646,-2.00647347901961,3.38314868003774));
#25078=CARTESIAN_POINT('Ctrl Pts',(-5.646,-1.90386409072627,3.45234035730095));
#25079=CARTESIAN_POINT('Ctrl Pts',(-5.646,-1.79775511151038,3.51657830519508));
#25080=CARTESIAN_POINT('Ctrl Pts',(-5.646,-1.68832072772984,3.57542852261345));
#25081=CARTESIAN_POINT('Ctrl Pts',(-5.646,-2.05008858490001,-2.87251537181987));
#25082=CARTESIAN_POINT('Ctrl Pts',(-5.61008344114424,-1.18607795770181,
-3.48068169523233));
#25083=CARTESIAN_POINT('Ctrl Pts',(-5.53459414563446,1.25030204642021,-3.90746250366534));
#25084=CARTESIAN_POINT('Ctrl Pts',(-5.41953211347069,3.98315669070171,-1.20222141896168));
#25085=CARTESIAN_POINT('Ctrl Pts',(-5.30081390350864,3.17803017110567,2.68595570733295));
#25086=CARTESIAN_POINT('Ctrl Pts',(-5.18209569354661,-0.520477180563039,
4.12779813317261));
#25087=CARTESIAN_POINT('Ctrl Pts',(-5.08501265836025,-3.1573187910564,2.23479178678414));
#25088=CARTESIAN_POINT('Ctrl Pts',(-5.02750235982792,-3.51942846575801,
0.532373395398288));
#25089=CARTESIAN_POINT('Ctrl Pts',(-5.0095647979496,-3.51824182757685,0.000900848728238278));
#25090=CARTESIAN_POINT('Origin',(-5.646,-9.39637619619865E-16,-2.12715743287418E-16));
#25091=CARTESIAN_POINT('',(-5.646,-3.954,-4.84225344382864E-16));
#25092=CARTESIAN_POINT('Origin',(-5.646,0.,0.));
#25093=CARTESIAN_POINT('Origin',(-5.646,0.,0.));
#25094=CARTESIAN_POINT('',(-5.646,2.04569608541843,-2.86913603522101));
#25095=CARTESIAN_POINT('Ctrl Pts',(-5.646,1.69249901178079,3.58003443294051));
#25096=CARTESIAN_POINT('Ctrl Pts',(-5.646,1.79910683175878,3.52349759682845));
#25097=CARTESIAN_POINT('Ctrl Pts',(-5.646,1.90274240538976,3.46193012866522));
#25098=CARTESIAN_POINT('Ctrl Pts',(-5.646,2.00300255842392,3.3953141034615));
#25099=CARTESIAN_POINT('Ctrl Pts',(-5.646,2.10503185727917,3.32752260166971));
#25100=CARTESIAN_POINT('Ctrl Pts',(-5.646,2.20356614449629,3.25450231195095));
#25101=CARTESIAN_POINT('Ctrl Pts',(-5.646,2.29842061962347,3.17666297164194));
#25102=CARTESIAN_POINT('Ctrl Pts',(-5.646,2.35385455809869,3.13117285432428));
#25103=CARTESIAN_POINT('Ctrl Pts',(-5.646,2.40803103805464,3.08403610735246));
#25104=CARTESIAN_POINT('Ctrl Pts',(-5.646,2.46090694714461,3.03532931840981));
#25105=CARTESIAN_POINT('Ctrl Pts',(-5.646,2.48067509371497,3.0171198358806));
#25106=CARTESIAN_POINT('Ctrl Pts',(-5.646,2.50026140964636,2.99869087503606));
#25107=CARTESIAN_POINT('Ctrl Pts',(-5.646,2.51966346254713,2.98004633066214));
#25108=CARTESIAN_POINT('Ctrl Pts',(-5.646,2.5332676652907,2.96697327272226));
#25109=CARTESIAN_POINT('Ctrl Pts',(-5.646,2.54677877844966,2.95379656682823));
#25110=CARTESIAN_POINT('Ctrl Pts',(-5.646,2.5601903809623,2.94052341544533));
#25111=CARTESIAN_POINT('Ctrl Pts',(-5.646,2.64704277931223,2.85456761484802));
#25112=CARTESIAN_POINT('Ctrl Pts',(-5.646,2.72979795902533,2.76450027536008));
#25113=CARTESIAN_POINT('Ctrl Pts',(-5.646,2.80828101128637,2.67073206305303));
#25114=CARTESIAN_POINT('Ctrl Pts',(-5.646,2.88147991128195,2.58327713109399));
#25115=CARTESIAN_POINT('Ctrl Pts',(-5.646,2.95096248865815,2.49260198813964));
#25116=CARTESIAN_POINT('Ctrl Pts',(-5.646,3.01655400858887,2.39901735366309));
#25117=CARTESIAN_POINT('Ctrl Pts',(-5.646,3.04525029855856,2.35807407607961));
#25118=CARTESIAN_POINT('Ctrl Pts',(-5.646,3.07320138235663,2.3165736780614));
#25119=CARTESIAN_POINT('Ctrl Pts',(-5.646,3.10039051575116,2.27454131446345));
#25120=CARTESIAN_POINT('Ctrl Pts',(-5.646,3.11563505786325,2.25097439426627));
#25121=CARTESIAN_POINT('Ctrl Pts',(-5.646,3.13064004341249,2.22724023348114));
#25122=CARTESIAN_POINT('Ctrl Pts',(-5.646,3.14540233301013,2.2033432169401));
#25123=CARTESIAN_POINT('Ctrl Pts',(-5.646,3.15850930411529,2.182125810031));
#25124=CARTESIAN_POINT('Ctrl Pts',(-5.646,3.1714273968094,2.16077571267399));
#25125=CARTESIAN_POINT('Ctrl Pts',(-5.646,3.18413915338665,2.13932213297246));
#25126=CARTESIAN_POINT('Ctrl Pts',(-5.646,3.24649773775284,2.0340798046093));
#25127=CARTESIAN_POINT('Ctrl Pts',(-5.646,3.30396139749785,1.92624527420896));
#25128=CARTESIAN_POINT('Ctrl Pts',(-5.646,3.35635415521047,1.8162165162223));
#25129=CARTESIAN_POINT('Ctrl Pts',(-5.646,3.40862386086259,1.7064461768793));
#25130=CARTESIAN_POINT('Ctrl Pts',(-5.646,3.45584679995269,1.59449106356881));
#25131=CARTESIAN_POINT('Ctrl Pts',(-5.646,3.49780098019105,1.48072575857657));
#25132=CARTESIAN_POINT('Ctrl Pts',(-5.646,3.53864854028781,1.36996122674223));
#25133=CARTESIAN_POINT('Ctrl Pts',(-5.646,3.57450174328363,1.2574799650644));
#25134=CARTESIAN_POINT('Ctrl Pts',(-5.646,3.60510776453686,1.14362007387887));
#25135=CARTESIAN_POINT('Ctrl Pts',(-5.646,3.62669073740589,1.06332754183119));
#25136=CARTESIAN_POINT('Ctrl Pts',(-5.646,3.64566336814893,0.982349262158363));
#25137=CARTESIAN_POINT('Ctrl Pts',(-5.646,3.66192149868813,0.900804466306592));
#25138=CARTESIAN_POINT('Ctrl Pts',(-5.646,3.66778547684093,0.871392911257449));
#25139=CARTESIAN_POINT('Ctrl Pts',(-5.646,3.67329619980581,0.841907674560768));
#25140=CARTESIAN_POINT('Ctrl Pts',(-5.646,3.67844834487312,0.812354423083884));
#25141=CARTESIAN_POINT('Ctrl Pts',(-5.646,3.68152767470266,0.794691060029537));
#25142=CARTESIAN_POINT('Ctrl Pts',(-5.646,3.68447904596225,0.777002104932098));
#25143=CARTESIAN_POINT('Ctrl Pts',(-5.646,3.68729866107252,0.759306528355325));
#25144=CARTESIAN_POINT('Ctrl Pts',(-5.646,3.70576394677868,0.643420542344302));
#25145=CARTESIAN_POINT('Ctrl Pts',(-5.646,3.71861385866923,0.52707879665178));
#25146=CARTESIAN_POINT('Ctrl Pts',(-5.646,3.72564577564316,0.410622409434895));
#25147=CARTESIAN_POINT('Ctrl Pts',(-5.646,3.73068658626485,0.327140963930941));
#25148=CARTESIAN_POINT('Ctrl Pts',(-5.646,3.73273671488304,0.243600328307105));
#25149=CARTESIAN_POINT('Ctrl Pts',(-5.646,3.7317049764916,0.160125554237579));
#25150=CARTESIAN_POINT('Ctrl Pts',(-5.646,3.730253423903,0.0426849070845082));
#25151=CARTESIAN_POINT('Ctrl Pts',(-5.646,3.72270365442221,-0.0746261863591401));
#25152=CARTESIAN_POINT('Ctrl Pts',(-5.646,3.70927694293084,-0.191449747144352));
#25153=CARTESIAN_POINT('Ctrl Pts',(-5.646,3.69573214444074,-0.309300763065067));
#25154=CARTESIAN_POINT('Ctrl Pts',(-5.646,3.67620617301247,-0.426656441051207));
#25155=CARTESIAN_POINT('Ctrl Pts',(-5.646,3.65087713531433,-0.543130167681983));
#25156=CARTESIAN_POINT('Ctrl Pts',(-5.646,3.64410795568506,-0.574257744933452));
#25157=CARTESIAN_POINT('Ctrl Pts',(-5.646,3.63692405661425,-0.605322188393886));
#25158=CARTESIAN_POINT('Ctrl Pts',(-5.646,3.62932830866254,-0.636315774732953));
#25159=CARTESIAN_POINT('Ctrl Pts',(-5.646,3.62539844276379,-0.652351145944345));
#25160=CARTESIAN_POINT('Ctrl Pts',(-5.646,3.6213605487996,-0.668358452270878));
#25161=CARTESIAN_POINT('Ctrl Pts',(-5.646,3.61721597080615,-0.684334502599823));
#25162=CARTESIAN_POINT('Ctrl Pts',(-5.646,3.58784792720512,-0.797539114353967));
#25163=CARTESIAN_POINT('Ctrl Pts',(-5.646,3.55311857210295,-0.90921231416928));
#25164=CARTESIAN_POINT('Ctrl Pts',(-5.646,3.51327894740302,-1.0190143738027));
#25165=CARTESIAN_POINT('Ctrl Pts',(-5.646,3.47320242549391,-1.12946934625056));
#25166=CARTESIAN_POINT('Ctrl Pts',(-5.646,3.42795422369401,-1.23803164326406));
#25167=CARTESIAN_POINT('Ctrl Pts',(-5.646,3.37774022348495,-1.34433650746171));
#25168=CARTESIAN_POINT('Ctrl Pts',(-5.646,3.32790839941417,-1.44983229087888));
#25169=CARTESIAN_POINT('Ctrl Pts',(-5.646,3.27318555283625,-1.55310558042916));
#25170=CARTESIAN_POINT('Ctrl Pts',(-5.646,3.21373162439723,-1.65377022854507));
#25171=CARTESIAN_POINT('Ctrl Pts',(-5.646,3.17762547871062,-1.71490348829414));
#25172=CARTESIAN_POINT('Ctrl Pts',(-5.646,3.13977370288082,-1.77507403709529));
#25173=CARTESIAN_POINT('Ctrl Pts',(-5.646,3.10020581820815,-1.83418830757275));
#25174=CARTESIAN_POINT('Ctrl Pts',(-5.646,3.08642921800113,-1.85477049632594));
#25175=CARTESIAN_POINT('Ctrl Pts',(-5.646,3.07244454081104,-1.87522458253508));
#25176=CARTESIAN_POINT('Ctrl Pts',(-5.646,3.05825291307383,-1.89554643852077));
#25177=CARTESIAN_POINT('Ctrl Pts',(-5.646,3.04634228662547,-1.91260198985464));
#25178=CARTESIAN_POINT('Ctrl Pts',(-5.646,3.03428371887915,-1.92956725129706));
#25179=CARTESIAN_POINT('Ctrl Pts',(-5.646,3.02209343607064,-1.94641861659085));
#25180=CARTESIAN_POINT('Ctrl Pts',(-5.646,2.95436095457071,-2.04004932278038));
#25181=CARTESIAN_POINT('Ctrl Pts',(-5.646,2.88247755796715,-2.13029552606011));
#25182=CARTESIAN_POINT('Ctrl Pts',(-5.646,2.80663876729683,-2.21681622171986));
#25183=CARTESIAN_POINT('Ctrl Pts',(-5.646,2.73167582096858,-2.30233771023118));
#25184=CARTESIAN_POINT('Ctrl Pts',(-5.646,2.65284778055453,-2.38421985926057));
#25185=CARTESIAN_POINT('Ctrl Pts',(-5.646,2.57030739842824,-2.46209859964859));
#25186=CARTESIAN_POINT('Ctrl Pts',(-5.646,2.48978889553354,-2.53806965068848));
#25187=CARTESIAN_POINT('Ctrl Pts',(-5.646,2.40573718380752,-2.61023146648245));
#25188=CARTESIAN_POINT('Ctrl Pts',(-5.646,2.31826727017074,-2.6782052332885));
#25189=CARTESIAN_POINT('Ctrl Pts',(-5.646,2.23079735653395,-2.74617900009456));
#25190=CARTESIAN_POINT('Ctrl Pts',(-5.646,2.13990886542514,-2.80996531714783));
#25191=CARTESIAN_POINT('Ctrl Pts',(-5.646,2.0456960854184,-2.86913603522103));
#25192=CARTESIAN_POINT('Origin',(-5.646,0.,0.));
#25193=CARTESIAN_POINT('Origin',(-7.03243520205041,0.,0.));
#25194=CARTESIAN_POINT('Ctrl Pts',(-5.646,2.04569608541839,-2.86913603522103));
#25195=CARTESIAN_POINT('Ctrl Pts',(-5.60642726334599,2.99688291874876,-2.19093912940735));
#25196=CARTESIAN_POINT('Ctrl Pts',(-5.52728179003796,4.15588292084424,0.17368053733326));
#25197=CARTESIAN_POINT('Ctrl Pts',(-5.40856358007592,2.11478894550069,3.58630724545133));
#25198=CARTESIAN_POINT('Ctrl Pts',(-5.28984537011388,-1.85304107076213,
3.72388412481386));
#25199=CARTESIAN_POINT('Ctrl Pts',(-5.20613591077205,-3.46080642106957,
1.43446279409787));
#25200=CARTESIAN_POINT('Ctrl Pts',(-5.16199918808422,-3.52857683297957,
0.136750902370548));
#25201=CARTESIAN_POINT('Ctrl Pts',(-5.1574352020504,-3.52758964538326,0.0024499632266353));
#25202=CARTESIAN_POINT('Ctrl Pts',(-5.89440495331884,2.29547565001616,-3.2194576469));
#25203=CARTESIAN_POINT('Ctrl Pts',(-5.85483221666482,3.36280242943815,-2.45845287482839));
#25204=CARTESIAN_POINT('Ctrl Pts',(-5.7756867433568,4.66331637290333,0.194886937102771));
#25205=CARTESIAN_POINT('Ctrl Pts',(-5.65696853339476,2.37300475076541,4.02419548734008));
#25206=CARTESIAN_POINT('Ctrl Pts',(-5.53825032343272,-2.07929745123621,
4.17857050855309));
#25207=CARTESIAN_POINT('Ctrl Pts',(-5.41953211347068,-4.63786592085608,
0.535227138001458));
#25208=CARTESIAN_POINT('Ctrl Pts',(-5.30081390350864,-2.97522613263464,
-3.59840638997019));
#25209=CARTESIAN_POINT('Ctrl Pts',(-5.1820956935466,1.39596514616172,-4.45488062147499));
#25210=CARTESIAN_POINT('Ctrl Pts',(-5.06337748358457,4.49629836096393,-1.25703816033307));
#25211=CARTESIAN_POINT('Ctrl Pts',(-4.94465927362252,3.5038389764095,3.08550240959749));
#25212=CARTESIAN_POINT('Ctrl Pts',(-4.82594106366049,-0.67811856098812,
4.61915125015357));
#25213=CARTESIAN_POINT('Ctrl Pts',(-4.70722285369845,-4.24278039300494,
1.94822471606856));
#25214=CARTESIAN_POINT('Ctrl Pts',(-4.58850464373641,-3.94535535609007,
-2.49618760971672));
#25215=CARTESIAN_POINT('Ctrl Pts',(-4.46978643377437,-0.0565651229095746,
-4.66834792415271));
#25216=CARTESIAN_POINT('Ctrl Pts',(-4.35106822381233,3.88371186515834,-2.5910446357827));
#25217=CARTESIAN_POINT('Ctrl Pts',(-4.2323500138503,4.28874367012574,1.84483192149852));
#25218=CARTESIAN_POINT('Ctrl Pts',(-4.11363180388825,0.789837394669197,
4.60139866153259));
#25219=CARTESIAN_POINT('Ctrl Pts',(-3.99491359392622,-3.42803786777068,
3.16942868543038));
#25220=CARTESIAN_POINT('Ctrl Pts',(-3.87619538396417,-4.52545532779526,
-1.14759516447504));
#25221=CARTESIAN_POINT('Ctrl Pts',(-3.75747717400214,-1.5034626703308,-4.41999081254857));
#25222=CARTESIAN_POINT('Ctrl Pts',(-3.6387589640401,2.88709478481946,-3.66897858534264));
#25223=CARTESIAN_POINT('Ctrl Pts',(-3.52004075407806,4.64960133826196,0.421814252099659));
#25224=CARTESIAN_POINT('Ctrl Pts',(-3.40132254411602,2.17969083882637,4.12863990933018));
#25225=CARTESIAN_POINT('Ctrl Pts',(-3.28260433415398,-2.27433828109485,
4.07726688351253));
#25226=CARTESIAN_POINT('Ctrl Pts',(-3.16388612419194,-4.65809355158234,
0.3144586843738));
#25227=CARTESIAN_POINT('Ctrl Pts',(-3.0451679142299,-2.80170153293177,-3.73459345798));
#25228=CARTESIAN_POINT('Ctrl Pts',(-2.92644970426786,1.60501005627966,-4.38413760326885));
#25229=CARTESIAN_POINT('Ctrl Pts',(-2.80773149430583,4.55072071104292,-1.04290977799098));
#25230=CARTESIAN_POINT('Ctrl Pts',(-2.68901328434378,3.3540229184984,3.24765300716171));
#25231=CARTESIAN_POINT('Ctrl Pts',(-2.57029507438175,-0.89575893480859,
4.58195763048246));
#25232=CARTESIAN_POINT('Ctrl Pts',(-2.45157686441971,-4.33015359714177,
1.74541961151293));
#25233=CARTESIAN_POINT('Ctrl Pts',(-2.33285865445767,-3.82291659791893,
-2.67993068572906));
#25234=CARTESIAN_POINT('Ctrl Pts',(-2.21414044449563,0.164226774937983,
-4.66580639995998));
#25235=CARTESIAN_POINT('Ctrl Pts',(-2.09542223453359,4.00187857869148,-2.40451401256942));
#25236=CARTESIAN_POINT('Ctrl Pts',(-1.97670402457155,4.1967193464349,2.0455479760931));
#25237=CARTESIAN_POINT('Ctrl Pts',(-1.85798581460952,0.57139034901314,4.63359826316093));
#25238=CARTESIAN_POINT('Ctrl Pts',(-1.73926760464748,-3.57406114296456,
3.00379871855954));
#25239=CARTESIAN_POINT('Ctrl Pts',(-1.62054939468544,-4.46613322351616,
-1.36028446476434));
#25240=CARTESIAN_POINT('Ctrl Pts',(-1.5018311847234,-1.29279475375635,-4.48613436267166));
#25241=CARTESIAN_POINT('Ctrl Pts',(-1.38311297476136,3.05734278765604,-3.52836716825847));
#25242=CARTESIAN_POINT('Ctrl Pts',(-1.26439476479932,4.62445684929134,0.641185343188987));
#25243=CARTESIAN_POINT('Ctrl Pts',(-1.14567655483728,1.98204228209413,4.22708270409631));
#25244=CARTESIAN_POINT('Ctrl Pts',(-1.02695834487524,-2.46457632504579,
3.96517128675444));
#25245=CARTESIAN_POINT('Ctrl Pts',(-0.908240134913205,-4.6677520941769,
0.0938625728684425));
#25246=CARTESIAN_POINT('Ctrl Pts',(-0.789521924951166,-2.62198864448019,
-3.86288691828992));
#25247=CARTESIAN_POINT('Ctrl Pts',(-0.670803714989127,1.8105061821359,-4.30334604229383));
#25248=CARTESIAN_POINT('Ctrl Pts',(-0.552085505027087,4.59494203561066,
-0.826575758570605));
#25249=CARTESIAN_POINT('Ctrl Pts',(-0.433367295065051,3.19671586474552,
3.40260598297286));
#25250=CARTESIAN_POINT('Ctrl Pts',(-0.314649085103009,-1.11140164891628,
4.53447970224418));
#25251=CARTESIAN_POINT('Ctrl Pts',(-0.195930875140972,-4.40783774534056,
1.53872876298241));
#25252=CARTESIAN_POINT('Ctrl Pts',(-0.0772126651789329,-3.69192822260236,
-2.85768889042012));
#25253=CARTESIAN_POINT('Ctrl Pts',(0.0415055447831063,0.38465219730754,
-4.65282306587999));
#25254=CARTESIAN_POINT('Ctrl Pts',(0.160223754745145,4.11109324096666,-2.21260754752318));
#25255=CARTESIAN_POINT('Ctrl Pts',(0.278941964707184,4.09530784428149,2.24168986611549));
#25256=CARTESIAN_POINT('Ctrl Pts',(0.397660174669223,0.351665063214532,
4.65543246955561));
#25257=CARTESIAN_POINT('Ctrl Pts',(0.516378384631261,-3.71208972226839,
2.83145010358787));
#25258=CARTESIAN_POINT('Ctrl Pts',(0.635096594593301,-4.39682109636873,
-1.5699312219984));
#25259=CARTESIAN_POINT('Ctrl Pts',(0.753814804555339,-1.07923503423744,
-4.54224300716648));
#25260=CARTESIAN_POINT('Ctrl Pts',(0.872533014517378,3.22075197181392,-3.37986338944861));
#25261=CARTESIAN_POINT('Ctrl Pts',(0.991251224479416,4.58896816162396,0.859122230465463));
#25262=CARTESIAN_POINT('Ctrl Pts',(1.10996943444146,1.7799601967492,4.31607014461849));
#25263=CARTESIAN_POINT('Ctrl Pts',(1.22868764440349,-2.64930148668855,3.84420621558056));
#25264=CARTESIAN_POINT('Ctrl Pts',(1.34740585436553,-4.66696958885342,-0.126943499225333));
#25265=CARTESIAN_POINT('Ctrl Pts',(1.46612406432757,-2.43641076742186,-3.9825396881474));
#25266=CARTESIAN_POINT('Ctrl Pts',(1.58484227428961,2.01195248192434,-4.21292855455169));
#25267=CARTESIAN_POINT('Ctrl Pts',(1.70356048425165,4.62888517660782,-0.608392814765849));
#25268=CARTESIAN_POINT('Ctrl Pts',(1.82227869421369,3.03225824568999,3.5499478484512));
#25269=CARTESIAN_POINT('Ctrl Pts',(1.94099690417573,-1.32455832721829,4.47685883550902));
#25270=CARTESIAN_POINT('Ctrl Pts',(2.05971511413777,-4.47566223360264,1.32859601308357));
#25271=CARTESIAN_POINT('Ctrl Pts',(2.1784333240998,-3.55268156760687,-3.02905488138869));
#25272=CARTESIAN_POINT('Ctrl Pts',(2.29715153406185,0.60421721144437,-4.62943207712054));
#25273=CARTESIAN_POINT('Ctrl Pts',(2.41586974402388,4.21111201543463,-2.01575181724849));
#25274=CARTESIAN_POINT('Ctrl Pts',(2.53458795398592,3.98473576383927,2.43281743821001));
#25275=CARTESIAN_POINT('Ctrl Pts',(2.65330616394796,0.131153156369908,4.66685318441158));
#25276=CARTESIAN_POINT('Ctrl Pts',(2.77202437391,-3.84181492370588,2.65276796709946));
#25277=CARTESIAN_POINT('Ctrl Pts',(2.89074258387204,-4.31767395183015,-1.77606628281883));
#25278=CARTESIAN_POINT('Ctrl Pts',(3.00946079383408,-0.863261230747963,
-4.58819134766261));
#25279=CARTESIAN_POINT('Ctrl Pts',(3.12817900379611,3.37695682562491,-3.22379937234679));
#25280=CARTESIAN_POINT('Ctrl Pts',(3.24689721375816,4.54321465292177,1.07513739250159));
#25281=CARTESIAN_POINT('Ctrl Pts',(3.36561542372019,1.57389661224691,4.39540319529804));
#25282=CARTESIAN_POINT('Ctrl Pts',(3.48433363368224,-2.82810056545818,3.71464224211883));
#25283=CARTESIAN_POINT('Ctrl Pts',(3.60305184364427,-4.6557477852134,-0.34746561809583));
#25284=CARTESIAN_POINT('Ctrl Pts',(3.72177005360631,-2.2453830115206,-4.09328412486269));
#25285=CARTESIAN_POINT('Ctrl Pts',(3.84048826356835,2.20889835123907,-4.11308738895392));
#25286=CARTESIAN_POINT('Ctrl Pts',(3.9592064735304,4.6524742083031,-0.388848989137025));
#25287=CARTESIAN_POINT('Ctrl Pts',(4.07792468349242,2.86101792796951,3.68934902267531));
#25288=CARTESIAN_POINT('Ctrl Pts',(4.19664289345447,-1.53475217080446,4.4092239191823));
#25289=CARTESIAN_POINT('Ctrl Pts',(4.3153611034165,-4.5334753488889,1.11549139678222));
#25290=CARTESIAN_POINT('Ctrl Pts',(4.43407931337854,-3.40548810644487,-3.1936453391291));
#25291=CARTESIAN_POINT('Ctrl Pts',(4.55279752334059,0.822430683944178,-4.59568575572627));
#25292=CARTESIAN_POINT('Ctrl Pts',(4.67151573330262,4.30171117536757,-1.81438715796713));
#25293=CARTESIAN_POINT('Ctrl Pts',(4.79023394326467,3.86525043796889,2.61850316919032));
#25294=CARTESIAN_POINT('Ctrl Pts',(4.9089521532267,-0.0896521200581657,
4.66783486132999));
#25295=CARTESIAN_POINT('Ctrl Pts',(5.02767036318874,-3.96294657181035,2.46815199375055));
#25296=CARTESIAN_POINT('Ctrl Pts',(5.14638857315078,-4.22886882997703,-1.97822855457275));
#25297=CARTESIAN_POINT('Ctrl Pts',(5.26510678311281,-0.645356443706703,
-4.62387660473814));
#25298=CARTESIAN_POINT('Ctrl Pts',(5.38382499307485,3.52560794268368,-3.06052420832841));
#25299=CARTESIAN_POINT('Ctrl Pts',(5.5025432030369,4.48729866679715,1.28874763636593));
#25300=CARTESIAN_POINT('Ctrl Pts',(5.62126141299893,1.36431246135956,4.46490440021477));
#25301=CARTESIAN_POINT('Ctrl Pts',(5.73997962296097,-3.00057361511833,3.57676918119331));
#25302=CARTESIAN_POINT('Ctrl Pts',(5.85869783292301,-4.63411178471802,-0.567210509437168));
#25303=CARTESIAN_POINT('Ctrl Pts',(5.97741604288506,-2.04933267669613,-4.19487251004172));
#25304=CARTESIAN_POINT('Ctrl Pts',(6.09613425284708,2.40090325224437,-4.00404587494208));
#25305=CARTESIAN_POINT('Ctrl Pts',(6.21485246280913,4.66565636563465,-0.168435367697401));
#25306=CARTESIAN_POINT('Ctrl Pts',(6.33357067277117,2.68337795002623,3.82049768650519));
#25307=CARTESIAN_POINT('Ctrl Pts',(6.4522888827332,-1.7415130081437,4.33172624224391));
#25308=CARTESIAN_POINT('Ctrl Pts',(6.57100709269525,-4.58114777208862,0.899891596563583));
#25309=CARTESIAN_POINT('Ctrl Pts',(6.68972530265728,-3.25067708841222,-3.35109209992061));
#25310=CARTESIAN_POINT('Ctrl Pts',(6.80844351261933,1.03880450459045,-4.55165958706503));
#25311=CARTESIAN_POINT('Ctrl Pts',(6.92716172258136,4.38268806427942,-1.6089639916732));
#25312=CARTESIAN_POINT('Ctrl Pts',(7.0458799325434,3.73711913709867,2.79833170843078));
#25313=CARTESIAN_POINT('Ctrl Pts',(7.16459814250544,-0.310256858383678,
4.65837530444943));
#25314=CARTESIAN_POINT('Ctrl Pts',(7.28331635246748,-4.07521371358196,2.27801514128243));
#25315=CARTESIAN_POINT('Ctrl Pts',(7.40203456242951,-4.13060437430629,-2.1759658311288));
#25316=CARTESIAN_POINT('Ctrl Pts',(7.52075277239156,-0.426008092847812,
-4.64921895592221));
#25317=CARTESIAN_POINT('Ctrl Pts',(7.63947098235358,3.66637281314061,-2.89040311900293));
#25318=CARTESIAN_POINT('Ctrl Pts',(7.75818919231564,4.42134527877262,1.4994751485615));
#25319=CARTESIAN_POINT('Ctrl Pts',(7.87690740227767,1.1516765518288,4.52441829578632));
#25320=CARTESIAN_POINT('Ctrl Pts',(7.99562561223971,-3.16633483979384,3.4308954337878));
#25321=CARTESIAN_POINT('Ctrl Pts',(8.11434382220175,-4.6021099837965,-0.785686637482825));
#25322=CARTESIAN_POINT('Ctrl Pts',(8.23306203216379,-1.84869829761031,-4.28707760597953));
#25323=CARTESIAN_POINT('Ctrl Pts',(8.35178024212583,2.58753769929621,-3.8860479217322));
#25324=CARTESIAN_POINT('Ctrl Pts',(8.47049845208786,4.66840216212944,0.0523550179394298));
#25325=CARTESIAN_POINT('Ctrl Pts',(8.58921666204991,2.49973566536485,3.94310048040643));
#25326=CARTESIAN_POINT('Ctrl Pts',(8.70793487201194,-1.94437834681552,4.24453915516319));
#25327=CARTESIAN_POINT('Ctrl Pts',(8.82665308197398,-4.6185728672708,0.682278876258279));
#25328=CARTESIAN_POINT('Ctrl Pts',(8.94537129193602,-3.08859480211636,-3.50104297940172));
#25329=CARTESIAN_POINT('Ctrl Pts',(9.06408950189806,1.25285467818704,-4.49745205095322));
#25330=CARTESIAN_POINT('Ctrl Pts',(9.18280771186011,4.45386154923497,-1.39994181862131));
#25331=CARTESIAN_POINT('Ctrl Pts',(9.30152592182213,3.60062847138283,2.97190080694926));
#25332=CARTESIAN_POINT('Ctrl Pts',(9.42024413178418,-0.530167599493716,
4.63849567335416));
#25333=CARTESIAN_POINT('Ctrl Pts',(9.53896234174621,-4.17836522456791,2.08278271679982));
#25334=CARTESIAN_POINT('Ctrl Pts',(9.65768055170827,-4.02310038740015,-2.36883580439405));
#25335=CARTESIAN_POINT('Ctrl Pts',(9.77639876167028,-0.205706826937308,
-4.66416171424508));
#25336=CARTESIAN_POINT('Ctrl Pts',(9.89511697163234,3.79893656747558,-2.71381663926939));
#25337=CARTESIAN_POINT('Ctrl Pts',(10.0138351815944,4.34550201650593,1.70684856382205));
#25338=CARTESIAN_POINT('Ctrl Pts',(10.1325533915564,0.936464517714484,4.57381175851606));
#25339=CARTESIAN_POINT('Ctrl Pts',(10.2512716015184,-3.32501345693721,3.27734729720019));
#25340=CARTESIAN_POINT('Ctrl Pts',(10.3699898114805,-4.55981396559068,-1.00240530449618));
#25341=CARTESIAN_POINT('Ctrl Pts',(10.4887080214425,-1.64392866273208,-4.3696931639561));
#25342=CARTESIAN_POINT('Ctrl Pts',(10.6074262314046,2.76838421963613,-3.75935747272765));
#25343=CARTESIAN_POINT('Ctrl Pts',(10.7261444413666,4.66070545585953,0.273028293396762));
#25344=CARTESIAN_POINT('Ctrl Pts',(10.8448626513287,2.31050185373462,4.05688316064908));
#25345=CARTESIAN_POINT('Ctrl Pts',(10.9635808612907,-2.14289440803709,4.14785768214349));
#25346=CARTESIAN_POINT('Ctrl Pts',(11.0822990712527,-4.64566692020879,0.463140002285691));
#25347=CARTESIAN_POINT('Ctrl Pts',(11.2010172812147,-2.91960380088829,-3.64316256034107));
#25348=CARTESIAN_POINT('Ctrl Pts',(11.3197354911768,1.46410240719433,-4.43318440139384));
#25349=CARTESIAN_POINT('Ctrl Pts',(11.4384537011388,4.51507242599213,-1.18778818945209));
#25350=CARTESIAN_POINT('Ctrl Pts',(11.5571719111009,3.45608374964487,3.13882221709585));
#25351=CARTESIAN_POINT('Ctrl Pts',(11.6758901210629,-0.748892436729798,
4.60824043589683));
#25352=CARTESIAN_POINT('Ctrl Pts',(11.794608331025,-4.27217037042104,1.882891425132));
#25353=CARTESIAN_POINT('Ctrl Pts',(11.913326540987,-3.90659733958176,-2.55640705313474));
#25354=CARTESIAN_POINT('Ctrl Pts',(12.032044750949,0.0150545743428436,-4.66867145609391));
#25355=CARTESIAN_POINT('Ctrl Pts',(12.150762960911,3.92300267965357,-2.53115976411015));
#25356=CARTESIAN_POINT('Ctrl Pts',(12.2694811708731,4.2599385319979,1.91040401566542));
#25357=CARTESIAN_POINT('Ctrl Pts',(12.3881993808351,0.719157751281456,4.61297431003179));
#25358=CARTESIAN_POINT('Ctrl Pts',(12.5069175907972,-3.47625451873963,3.11646822135571));
#25359=CARTESIAN_POINT('Ctrl Pts',(12.6256358007592,-4.50731835499655,-1.21688171765083));
#25360=CARTESIAN_POINT('Ctrl Pts',(12.7443540107213,-1.4354817816321,-4.44253443552631));
#25361=CARTESIAN_POINT('Ctrl Pts',(12.8630722206833,2.94303823237952,-3.62425782013981));
#25362=CARTESIAN_POINT('Ctrl Pts',(12.9817904306454,4.64258356746131,0.493090665633712));
#25363=CARTESIAN_POINT('Ctrl Pts',(13.1005086406074,2.11609960396394,4.1615915562441));
#25364=CARTESIAN_POINT('Ctrl Pts',(13.2192268505694,-2.33661676455732,4.04189743164783));
#25365=CARTESIAN_POINT('Ctrl Pts',(13.3379450605315,-4.66237004285371,0.242966397108652));
#25366=CARTESIAN_POINT('Ctrl Pts',(13.4566632704935,-2.74408072785275,-3.77713530538915));
#25367=CARTESIAN_POINT('Ctrl Pts',(13.5753814804556,1.67207256885561,-4.35899590256187));
#25368=CARTESIAN_POINT('Ctrl Pts',(13.6940996904176,4.56618870795816,-0.972986203420864));
#25369=CARTESIAN_POINT('Ctrl Pts',(13.8128179003796,3.30379891551882,3.29873880951256));
#25370=CARTESIAN_POINT('Ctrl Pts',(13.9315361103416,-0.965924276211378,
4.56764636844593));
#25371=CARTESIAN_POINT('Ctrl Pts',(14.0502543203037,-4.35645324991307,1.67884715610445));
#25372=CARTESIAN_POINT('Ctrl Pts',(14.1689725302657,-3.78129131083658,-2.73837176255018));
#25373=CARTESIAN_POINT('Ctrl Pts',(14.2876907402277,0.235659599280402,-4.66252555962526));
#25374=CARTESIAN_POINT('Ctrl Pts',(14.4064089501898,4.03852700863023,-2.34324533249394));
#25375=CARTESIAN_POINT('Ctrl Pts',(14.5251271601518,4.16440214623227,2.11045567438585));
#25376=CARTESIAN_POINT('Ctrl Pts',(14.6438453701139,0.501089014228282,4.64034903703233));
#25377=CARTESIAN_POINT('Ctrl Pts',(14.7625635800759,-3.6213485503704,2.95146328864409));
#25378=CARTESIAN_POINT('Ctrl Pts',(14.881281790038,-4.44148208883051,-1.43448156720096));
#25379=CARTESIAN_POINT('Ctrl Pts',(14.960427263346,-2.30148466178617,-3.47211737542815));
#25380=CARTESIAN_POINT('Ctrl Pts',(15.,-1.03647793659398,-3.81573446232228));
#25381=CARTESIAN_POINT('Ctrl Pts',(-5.81160330221256,2.21221579515024,-3.10268377634035));
#25382=CARTESIAN_POINT('Ctrl Pts',(-5.77203056555854,3.24082925920835,-2.36928162635471));
#25383=CARTESIAN_POINT('Ctrl Pts',(-5.69288509225051,4.49417188888364,0.187818137179599));
#25384=CARTESIAN_POINT('Ctrl Pts',(-5.57416688228849,2.28693281567717,3.87823274004383));
#25385=CARTESIAN_POINT('Ctrl Pts',(-5.45544867232644,-2.00387865774485,
4.02700838064001));
#25386=CARTESIAN_POINT('Ctrl Pts',(-5.33673046236441,-4.46964455747315,
0.515813761157338));
#25387=CARTESIAN_POINT('Ctrl Pts',(-5.21801225240236,-2.8673108532917,-3.46788756099659));
#25388=CARTESIAN_POINT('Ctrl Pts',(-5.09929404244033,1.34533169445575,-4.29329637030406));
#25389=CARTESIAN_POINT('Ctrl Pts',(-4.98057583247828,4.33321183509941,-1.21144376912727));
#25390=CARTESIAN_POINT('Ctrl Pts',(-4.86185762251625,3.37675022918306,2.97358726782297));
#25391=CARTESIAN_POINT('Ctrl Pts',(-4.74313941255421,-0.653522328408015,
4.45160869195271));
#25392=CARTESIAN_POINT('Ctrl Pts',(-4.62442120259217,-4.08888928997927,
1.87756009930171));
#25393=CARTESIAN_POINT('Ctrl Pts',(-4.50570299263013,-3.80225224177903,
-2.40564767386436));
#25394=CARTESIAN_POINT('Ctrl Pts',(-4.3869847826681,-0.0545134331328301,
-4.4990209392963));
#25395=CARTESIAN_POINT('Ctrl Pts',(-4.26826657270605,3.74284463956531,-2.49706411356509));
#25396=CARTESIAN_POINT('Ctrl Pts',(-4.14954836274402,4.13318541990895,1.7779174944015));
#25397=CARTESIAN_POINT('Ctrl Pts',(-4.03083015278198,0.761188976269582,
4.43450001255902));
#25398=CARTESIAN_POINT('Ctrl Pts',(-3.91211194281993,-3.30369852426972,
3.05446942966354));
#25399=CARTESIAN_POINT('Ctrl Pts',(-3.7933937328579,-4.36131124123449,-1.10597041152313));
#25400=CARTESIAN_POINT('Ctrl Pts',(-3.67467552289586,-1.44893014513188,
-4.25967205963177));
#25401=CARTESIAN_POINT('Ctrl Pts',(-3.55595731293382,2.78237614283929,-3.53590001205453));
#25402=CARTESIAN_POINT('Ctrl Pts',(-3.43723910297178,4.48095431619256,0.406514506528419));
#25403=CARTESIAN_POINT('Ctrl Pts',(-3.31852089300974,2.10063064801496,3.97888882848467));
#25404=CARTESIAN_POINT('Ctrl Pts',(-3.1998026830477,-2.19184510579209,3.92937916840284));
#25405=CARTESIAN_POINT('Ctrl Pts',(-3.08108447308566,-4.48913850601091,
0.30305286335275));
#25406=CARTESIAN_POINT('Ctrl Pts',(-2.96236626312363,-2.70008021405268,
-3.59913494885035));
#25407=CARTESIAN_POINT('Ctrl Pts',(-2.84364805316158,1.54679427675559,-4.2251192923764));
#25408=CARTESIAN_POINT('Ctrl Pts',(-2.72492984319955,4.38566021652883,-1.00508209868054));
#25409=CARTESIAN_POINT('Ctrl Pts',(-2.60621163323751,3.23236819242489,3.12985645461311));
#25410=CARTESIAN_POINT('Ctrl Pts',(-2.48749342327547,-0.863268605884161,
4.41576413271522));
#25411=CARTESIAN_POINT('Ctrl Pts',(-2.36877521331343,-4.17309335559985,
1.68211099678916));
#25412=CARTESIAN_POINT('Ctrl Pts',(-2.25005700335139,-3.68425449487943,
-2.58272615213143));
#25413=CARTESIAN_POINT('Ctrl Pts',(-2.13133879338935,0.158270058539632,
-4.49657159945561));
#25414=CARTESIAN_POINT('Ctrl Pts',(-2.01262058342732,3.85672529438174,-2.31729919602012));
#25415=CARTESIAN_POINT('Ctrl Pts',(-1.89390237346527,4.04449893682408,1.97135331948257));
#25416=CARTESIAN_POINT('Ctrl Pts',(-1.77518416350324,0.550665285983065,
4.46553169321277));
#25417=CARTESIAN_POINT('Ctrl Pts',(-1.6564659535412,-3.44442534741907,2.89484707476759));
#25418=CARTESIAN_POINT('Ctrl Pts',(-1.53774774357916,-4.30414082599316,
-1.31094519727446));
#25419=CARTESIAN_POINT('Ctrl Pts',(-1.41902953361712,-1.24590342490763,
-4.3234164981008));
#25420=CARTESIAN_POINT('Ctrl Pts',(-1.30031132365508,2.94644903159558,-3.4003887519591));
#25421=CARTESIAN_POINT('Ctrl Pts',(-1.18159311369304,4.45672185018431,0.617928725931589));
#25422=CARTESIAN_POINT('Ctrl Pts',(-1.062874903731,1.91015105870255,4.07376097644183));
#25423=CARTESIAN_POINT('Ctrl Pts',(-0.944156693768964,-2.37518297115512,
3.82134942314577));
#25424=CARTESIAN_POINT('Ctrl Pts',(-0.825438483806927,-4.49844672084023,
0.0904580565999837));
#25425=CARTESIAN_POINT('Ctrl Pts',(-0.706720273844886,-2.52688574325886,
-3.7227750403103));
#25426=CARTESIAN_POINT('Ctrl Pts',(-0.588002063882848,1.74483679376428,
-4.14725814525313));
#25427=CARTESIAN_POINT('Ctrl Pts',(-0.469283853920809,4.42827757676548,
-0.79659479244981));
#25428=CARTESIAN_POINT('Ctrl Pts',(-0.350565643958771,3.08076686788102,
3.27918908665064));
#25429=CARTESIAN_POINT('Ctrl Pts',(-0.231847433996731,-1.07108968133524,
4.37000829001264));
#25430=CARTESIAN_POINT('Ctrl Pts',(-0.113129224034693,-4.24795979980585,
1.48291709123456));
#25431=CARTESIAN_POINT('Ctrl Pts',(0.00558898592734578,-3.55801723644702,
-2.75403683805935));
#25432=CARTESIAN_POINT('Ctrl Pts',(0.124307195889386,0.370700367271144,
-4.48405918760526));
#25433=CARTESIAN_POINT('Ctrl Pts',(0.243025405851424,3.9619786003558,-2.13235342534128));
#25434=CARTESIAN_POINT('Ctrl Pts',(0.361743615813462,3.94676576031572,2.16038089082496));
#25435=CARTESIAN_POINT('Ctrl Pts',(0.480461825775502,0.338909718968374,
4.48657394485266));
#25436=CARTESIAN_POINT('Ctrl Pts',(0.59918003573754,-3.57744745258317,2.72874976578071));
#25437=CARTESIAN_POINT('Ctrl Pts',(0.71789824569958,-4.23734273886472,-1.51298779692127));
#25438=CARTESIAN_POINT('Ctrl Pts',(0.836616455661619,-1.04008979115191,
-4.37749000987822));
#25439=CARTESIAN_POINT('Ctrl Pts',(0.955334665623656,3.10393115442452,-3.25727139625099));
#25440=CARTESIAN_POINT('Ctrl Pts',(1.0740528755857,4.42252038287345,0.827960761939252));
#25441=CARTESIAN_POINT('Ctrl Pts',(1.19277108554773,1.71539875056379,4.15952072801739));
#25442=CARTESIAN_POINT('Ctrl Pts',(1.31148929550978,-2.55320791354339,3.70477191072022));
#25443=CARTESIAN_POINT('Ctrl Pts',(1.43020750547181,-4.4976925979915,-0.122339095200565));
#25444=CARTESIAN_POINT('Ctrl Pts',(1.54892571543385,-2.34803901454013,-3.83808785027642));
#25445=CARTESIAN_POINT('Ctrl Pts',(1.66764392539589,1.93897637710659,-4.06012021610996));
#25446=CARTESIAN_POINT('Ctrl Pts',(1.78636213535793,4.46098955637215,-0.586325624700695));
#25447=CARTESIAN_POINT('Ctrl Pts',(1.90508034531997,2.92227433823694,3.42118667311853));
#25448=CARTESIAN_POINT('Ctrl Pts',(2.02379855528201,-1.27651489269748,4.31447740624096));
#25449=CARTESIAN_POINT('Ctrl Pts',(2.14251676524405,-4.31332420662509,1.28040612650213));
#25450=CARTESIAN_POINT('Ctrl Pts',(2.26123497520609,-3.42382123676361,-2.91918716407984));
#25451=CARTESIAN_POINT('Ctrl Pts',(2.37995318516812,0.582301475883412,-4.46151662009971));
#25452=CARTESIAN_POINT('Ctrl Pts',(2.49867139513016,4.05836956520357,-1.94263790565087));
#25453=CARTESIAN_POINT('Ctrl Pts',(2.6173896050922,3.8402042714778,2.34457602000145));
#25454=CARTESIAN_POINT('Ctrl Pts',(2.73610781505424,0.126396062664967,4.4975804156885));
#25455=CARTESIAN_POINT('Ctrl Pts',(2.85482602501628,-3.70246735407811,2.55654866025033));
#25456=CARTESIAN_POINT('Ctrl Pts',(2.97354423497832,-4.16106636307827,-1.71164607390103));
#25457=CARTESIAN_POINT('Ctrl Pts',(3.09226244494036,-0.831949635356866,
-4.4217717449538));
#25458=CARTESIAN_POINT('Ctrl Pts',(3.2109806549024,3.25447025723634,-3.10686802181972));
#25459=CARTESIAN_POINT('Ctrl Pts',(3.32969886486444,4.37842641279199,1.03614077615325));
#25460=CARTESIAN_POINT('Ctrl Pts',(3.44841707482647,1.51680935736416,4.23597626688993));
#25461=CARTESIAN_POINT('Ctrl Pts',(3.56713528478851,-2.72552171970801,3.57990738925493));
#25462=CARTESIAN_POINT('Ctrl Pts',(3.68585349475055,-4.48687782360591,-0.334862593126525));
#25463=CARTESIAN_POINT('Ctrl Pts',(3.80457170471259,-2.16394008109515,-3.94481544380366));
#25464=CARTESIAN_POINT('Ctrl Pts',(3.92328991467463,2.1287787663781,-3.96390041803019));
#25465=CARTESIAN_POINT('Ctrl Pts',(4.04200812463667,4.48372298354147,-0.374744936061991));
#25466=CARTESIAN_POINT('Ctrl Pts',(4.16072633459871,2.75724512713418,3.55553158741935));
#25467=CARTESIAN_POINT('Ctrl Pts',(4.27944454456074,-1.47908473517061,4.24929569533909));
#25468=CARTESIAN_POINT('Ctrl Pts',(4.39816275452279,-4.36904036584561,1.0750310887848));
#25469=CARTESIAN_POINT('Ctrl Pts',(4.51688096448482,-3.28196667179659,-3.0778077141788));
#25470=CARTESIAN_POINT('Ctrl Pts',(4.63559917444687,0.792600065012534,-4.42899432119574));
#25471=CARTESIAN_POINT('Ctrl Pts',(4.7543173844089,4.14568257705346,-1.74857700160942));
#25472=CARTESIAN_POINT('Ctrl Pts',(4.87303559437094,3.72505283208995,2.52352669064166));
#25473=CARTESIAN_POINT('Ctrl Pts',(4.99175380433298,-0.0864003223296886,
4.4985264859222));
#25474=CARTESIAN_POINT('Ctrl Pts',(5.11047201429502,-3.8192054014747,2.37862894575603));
#25475=CARTESIAN_POINT('Ctrl Pts',(5.22919022425706,-4.07548231723908,-1.90647565998456));
#25476=CARTESIAN_POINT('Ctrl Pts',(5.34790843421909,-0.6219485352676,-4.45616265184752));
#25477=CARTESIAN_POINT('Ctrl Pts',(5.46662664418114,3.39772960704553,-2.94951505804741));
#25478=CARTESIAN_POINT('Ctrl Pts',(5.58534485414316,4.32453857141784,1.24200310167139));
#25479=CARTESIAN_POINT('Ctrl Pts',(5.70406306410522,1.31482709325133,4.30295657369375));
#25480=CARTESIAN_POINT('Ctrl Pts',(5.82278127406724,-2.89173894997714,3.44703516161749));
#25481=CARTESIAN_POINT('Ctrl Pts',(5.9414994840293,-4.46602658868237,-0.54663705456568));
#25482=CARTESIAN_POINT('Ctrl Pts',(6.06021769399132,-1.97500074412587,-4.04271908756276));
#25483=CARTESIAN_POINT('Ctrl Pts',(6.17893590395337,2.31381940261713,-3.8588139800092));
#25484=CARTESIAN_POINT('Ctrl Pts',(6.2976541139154,4.49642700706827,-0.162326000225504));
#25485=CARTESIAN_POINT('Ctrl Pts',(6.41637232387745,2.5860483797178,3.68192332049448));
#25486=CARTESIAN_POINT('Ctrl Pts',(6.53509053383948,-1.67834609094981,4.17460895884099));
#25487=CARTESIAN_POINT('Ctrl Pts',(6.65380874380152,-4.41498364892716,0.86725137068082));
#25488=CARTESIAN_POINT('Ctrl Pts',(6.77252695376356,-3.13277084854633,-3.2295436784073));
#25489=CARTESIAN_POINT('Ctrl Pts',(6.8912451637256,1.00112572882749,-4.38656503830979));
#25490=CARTESIAN_POINT('Ctrl Pts',(7.00996337368764,4.22372233003087,-1.55060479782585));
#25491=CARTESIAN_POINT('Ctrl Pts',(7.12868158364969,3.60156901833821,2.69683261742147));
#25492=CARTESIAN_POINT('Ctrl Pts',(7.24739979361171,-0.299003442996754,
4.48941003933905));
#25493=CARTESIAN_POINT('Ctrl Pts',(7.36611800357376,-3.92740046958695,2.19538860153057));
#25494=CARTESIAN_POINT('Ctrl Pts',(7.48483621353579,-3.9807820397889,-2.09704075113864));
#25495=CARTESIAN_POINT('Ctrl Pts',(7.60355442349784,-0.410556231277453,
-4.48058580335219));
#25496=CARTESIAN_POINT('Ctrl Pts',(7.72227263345987,3.53338875456248,-2.78556447948591));
#25497=CARTESIAN_POINT('Ctrl Pts',(7.84099084342191,4.26097739762341,1.44508725590692));
#25498=CARTESIAN_POINT('Ctrl Pts',(7.95970905338396,1.10990376170705,4.3603118237106));
#25499=CARTESIAN_POINT('Ctrl Pts',(8.07842726334598,-3.05148780178832,3.30645244269127));
#25500=CARTESIAN_POINT('Ctrl Pts',(8.19714547330804,-4.43518553424934,-0.757188772386117));
#25501=CARTESIAN_POINT('Ctrl Pts',(8.31586368327006,-1.7816436320778,-4.13157978605264));
#25502=CARTESIAN_POINT('Ctrl Pts',(8.43458189323211,2.49368437817648,-3.74509596436201));
#25503=CARTESIAN_POINT('Ctrl Pts',(8.55330010319414,4.49907320999184,0.0504560340860681));
#25504=CARTESIAN_POINT('Ctrl Pts',(8.67201831315618,2.40906703696972,3.80007915333722));
#25505=CARTESIAN_POINT('Ctrl Pts',(8.79073652311823,-1.87385324280966,4.09058425957148));
#25506=CARTESIAN_POINT('Ctrl Pts',(8.90945473308026,-4.45105128776116,0.65753174369126));
#25507=CARTESIAN_POINT('Ctrl Pts',(9.02817294304229,-2.97656749528695,-3.37405564658367));
#25508=CARTESIAN_POINT('Ctrl Pts',(9.14689115300435,1.20741202726054,-4.33432367926863));
#25509=CARTESIAN_POINT('Ctrl Pts',(9.26560936296637,4.29231426112518,-1.34916412788942));
#25510=CARTESIAN_POINT('Ctrl Pts',(9.38432757292842,3.47002904465779,2.86410614144681));
#25511=CARTESIAN_POINT('Ctrl Pts',(9.50304578289045,-0.510937738620143,
4.47025146803797));
#25512=CARTESIAN_POINT('Ctrl Pts',(9.6217639928525,-4.02681054256906,2.00723750824284));
#25513=CARTESIAN_POINT('Ctrl Pts',(9.74048220281453,-3.87717736078754,-2.28291508235387));
#25514=CARTESIAN_POINT('Ctrl Pts',(9.85920041277658,-0.198245575690498,
-4.49498656860741));
#25515=CARTESIAN_POINT('Ctrl Pts',(9.9779186227386,3.66114425098962,-2.61538301854392));
#25516=CARTESIAN_POINT('Ctrl Pts',(10.0966368327007,4.18788506804854,1.64493897061816));
#25517=CARTESIAN_POINT('Ctrl Pts',(10.2153550426627,0.902497744931939,4.40791372200438));
#25518=CARTESIAN_POINT('Ctrl Pts',(10.3340732526247,-3.20441094135405,3.15847369455137));
#25519=CARTESIAN_POINT('Ctrl Pts',(10.4527914625868,-4.39442364703602,-0.966046774546791));
#25520=CARTESIAN_POINT('Ctrl Pts',(10.5715096725488,-1.58430125528474,-4.21119877145971));
#25521=CARTESIAN_POINT('Ctrl Pts',(10.6902278825109,2.66797136257167,-3.62300074092517));
#25522=CARTESIAN_POINT('Ctrl Pts',(10.8089460924729,4.49165567315985,0.263125205955005));
#25523=CARTESIAN_POINT('Ctrl Pts',(10.9276643024349,2.22669697912923,3.90973478939049));
#25524=CARTESIAN_POINT('Ctrl Pts',(11.046382512397,-2.06516887110756,3.99740954795515));
#25525=CARTESIAN_POINT('Ctrl Pts',(11.165100722359,-4.47716260454366,0.446341318591266));
#25526=CARTESIAN_POINT('Ctrl Pts',(11.283818932321,-2.81370601507375,-3.51102036749106));
#25527=CARTESIAN_POINT('Ctrl Pts',(11.4025371422831,1.41099752937478,-4.27238710003659));
#25528=CARTESIAN_POINT('Ctrl Pts',(11.5212553522451,4.35130494063695,-1.14470558377753));
#25529=CARTESIAN_POINT('Ctrl Pts',(11.6399735622072,3.33072714592842,3.02497309730951));
#25530=CARTESIAN_POINT('Ctrl Pts',(11.7586917721692,-0.721729144628708,
4.44109362696541));
#25531=CARTESIAN_POINT('Ctrl Pts',(11.8774099821313,-4.11721325510543,1.81459653087615));
#25532=CARTESIAN_POINT('Ctrl Pts',(11.9961281920933,-3.76490002839014,-2.46368288059964));
#25533=CARTESIAN_POINT('Ctrl Pts',(12.1148464020553,0.0145085255642979,
-4.49933273631779));
#25534=CARTESIAN_POINT('Ctrl Pts',(12.2335646120174,3.78071032567269,-2.43935134322764));
#25535=CARTESIAN_POINT('Ctrl Pts',(12.3522828219794,4.1054250811977,1.84111120435702));
#25536=CARTESIAN_POINT('Ctrl Pts',(12.4710010319414,0.69307297447411,4.44565579739554));
#25537=CARTESIAN_POINT('Ctrl Pts',(12.5897192419035,-3.35016629527918,3.00342990975242));
#25538=CARTESIAN_POINT('Ctrl Pts',(12.7084374518655,-4.3438321197717,-1.17274385228079));
#25539=CARTESIAN_POINT('Ctrl Pts',(12.8271556618276,-1.38341501072103,-4.28139799640262));
#25540=CARTESIAN_POINT('Ctrl Pts',(12.9458738717896,2.83629044958729,-3.49280132653712));
#25541=CARTESIAN_POINT('Ctrl Pts',(13.0645920817516,4.47419108896694,0.475205632849264));
#25542=CARTESIAN_POINT('Ctrl Pts',(13.1833102917137,2.03934594904864,4.01064527677402));
#25543=CARTESIAN_POINT('Ctrl Pts',(13.3020285016757,-2.25186466854054,3.89529261205869));
#25544=CARTESIAN_POINT('Ctrl Pts',(13.4207467116377,-4.49325988344233,0.234153693318749));
#25545=CARTESIAN_POINT('Ctrl Pts',(13.5394649215998,-2.64454938970079,-3.64013374872553));
#25546=CARTESIAN_POINT('Ctrl Pts',(13.6581831315618,1.61142434572711,-4.20088951349786));
#25547=CARTESIAN_POINT('Ctrl Pts',(13.7769013415238,4.40056716929698,-0.937694742114035));
#25548=CARTESIAN_POINT('Ctrl Pts',(13.8956195514859,3.18396587864461,3.17908930919281));
#25549=CARTESIAN_POINT('Ctrl Pts',(14.0143377614479,-0.930888960089293,
4.40197195856363));
#25550=CARTESIAN_POINT('Ctrl Pts',(14.13305597141,-4.19843908613166,1.61795320998123));
#25551=CARTESIAN_POINT('Ctrl Pts',(14.251774181372,-3.64413901050886,-2.63904749591409));
#25552=CARTESIAN_POINT('Ctrl Pts',(14.3704923913341,0.227111922447612,-4.4934097594205));
#25553=CARTESIAN_POINT('Ctrl Pts',(14.4892106012961,3.89204443861984,-2.25825280979074));
#25554=CARTESIAN_POINT('Ctrl Pts',(14.6079288112581,4.01335392304761,2.03390673205702));
#25555=CARTESIAN_POINT('Ctrl Pts',(14.7266470212201,0.48291387105078,4.47203760783125));
#25556=CARTESIAN_POINT('Ctrl Pts',(14.8453652311822,-3.48999757972489,2.84440991822266));
#25557=CARTESIAN_POINT('Ctrl Pts',(14.9640834411442,-4.28038381967528,-1.38245107535402));
#25558=CARTESIAN_POINT('Ctrl Pts',(15.0432289144523,-2.218006852333,-3.34617921147789));
#25559=CARTESIAN_POINT('Ctrl Pts',(15.0828016511063,-0.99888354844532,-3.6773328645804));
#25560=CARTESIAN_POINT('Ctrl Pts',(-5.72880165110628,2.12895594028432,-2.98590990578069));
#25561=CARTESIAN_POINT('Ctrl Pts',(-5.68922891445227,3.11885608897856,-2.28011037788103));
#25562=CARTESIAN_POINT('Ctrl Pts',(-5.61008344114424,4.32502740486394,0.180749337256433));
#25563=CARTESIAN_POINT('Ctrl Pts',(-5.4913652311822,2.20086088058893,3.73226999274757));
#25564=CARTESIAN_POINT('Ctrl Pts',(-5.37264702122016,-1.92845986425349,
3.87544625272694));
#25565=CARTESIAN_POINT('Ctrl Pts',(-5.25392881125813,-4.30142319409022,
0.496400384313214));
#25566=CARTESIAN_POINT('Ctrl Pts',(-5.13521060129608,-2.75939557394876,
-3.337368732023));
#25567=CARTESIAN_POINT('Ctrl Pts',(-5.01649239133405,1.29469824274977,-4.13171211913313));
#25568=CARTESIAN_POINT('Ctrl Pts',(-4.897774181372,4.17012530923491,-1.16584937792148));
#25569=CARTESIAN_POINT('Ctrl Pts',(-4.77905597140997,3.24966148195661,2.86167212604844));
#25570=CARTESIAN_POINT('Ctrl Pts',(-4.66033776144792,-0.628926095827896,
4.28406613375186));
#25571=CARTESIAN_POINT('Ctrl Pts',(-4.5416195514859,-3.93499818695361,1.80689548253486));
#25572=CARTESIAN_POINT('Ctrl Pts',(-4.42290134152385,-3.65914912746798,
-2.31510773801199));
#25573=CARTESIAN_POINT('Ctrl Pts',(-4.30418313156181,-0.0524617433560917,
-4.32969395443989));
#25574=CARTESIAN_POINT('Ctrl Pts',(-4.18546492159977,3.60197741397228,-2.40308359134747));
#25575=CARTESIAN_POINT('Ctrl Pts',(-4.06674671163773,3.97762716969217,1.71100306730448));
#25576=CARTESIAN_POINT('Ctrl Pts',(-3.9480285016757,0.732540557869959,4.26760136358546));
#25577=CARTESIAN_POINT('Ctrl Pts',(-3.82931029171366,-3.17935918076875,
2.93951017389669));
#25578=CARTESIAN_POINT('Ctrl Pts',(-3.71059208175161,-4.19716715467372,
-1.06434565857122));
#25579=CARTESIAN_POINT('Ctrl Pts',(-3.59187387178958,-1.39439761993295,
-4.09935330671497));
#25580=CARTESIAN_POINT('Ctrl Pts',(-3.47315566182754,2.67765750085913,-3.40282143876642));
#25581=CARTESIAN_POINT('Ctrl Pts',(-3.35443745186551,4.31230729412316,0.391214760957178));
#25582=CARTESIAN_POINT('Ctrl Pts',(-3.23571924190346,2.02157045720355,3.82913774763917));
#25583=CARTESIAN_POINT('Ctrl Pts',(-3.11700103194143,-2.10935193048935,
3.78149145329314));
#25584=CARTESIAN_POINT('Ctrl Pts',(-2.99828282197938,-4.32018346043948,
0.291647042331706));
#25585=CARTESIAN_POINT('Ctrl Pts',(-2.87956461201735,-2.59845889517359,
-3.46367643972069));
#25586=CARTESIAN_POINT('Ctrl Pts',(-2.76084640205531,1.48857849723153,-4.06610098148393));
#25587=CARTESIAN_POINT('Ctrl Pts',(-2.64212819209327,4.22059972201472,-0.967254419370101));
#25588=CARTESIAN_POINT('Ctrl Pts',(-2.52340998213123,3.1107134663514,3.01205990206451));
#25589=CARTESIAN_POINT('Ctrl Pts',(-2.40469177216919,-0.830778276959734,
4.24957063494798));
#25590=CARTESIAN_POINT('Ctrl Pts',(-2.28597356220715,-4.01603311405792,
1.6188023820654));
#25591=CARTESIAN_POINT('Ctrl Pts',(-2.16725535224512,-3.54559239183993,
-2.4855216185338));
#25592=CARTESIAN_POINT('Ctrl Pts',(-2.04853714228307,0.152313342141281,
-4.32733679895125));
#25593=CARTESIAN_POINT('Ctrl Pts',(-1.92981893232104,3.711572010072,-2.23008437947081));
#25594=CARTESIAN_POINT('Ctrl Pts',(-1.811100722359,3.89227852721326,1.89715866287202));
#25595=CARTESIAN_POINT('Ctrl Pts',(-1.69238251239696,0.529940222952991,
4.29746512326462));
#25596=CARTESIAN_POINT('Ctrl Pts',(-1.57366430243492,-3.31478955187358,
2.78589543097564));
#25597=CARTESIAN_POINT('Ctrl Pts',(-1.45494609247288,-4.14214842847016,
-1.26160592978457));
#25598=CARTESIAN_POINT('Ctrl Pts',(-1.33622788251084,-1.19901209605891,
-4.16069863352995));
#25599=CARTESIAN_POINT('Ctrl Pts',(-1.2175096725488,2.83555527553512,-3.27241033565973));
#25600=CARTESIAN_POINT('Ctrl Pts',(-1.09879146258676,4.28898685107728,0.594672108674195));
#25601=CARTESIAN_POINT('Ctrl Pts',(-0.980073252624725,1.83825983531098,
3.92043924878734));
#25602=CARTESIAN_POINT('Ctrl Pts',(-0.861355042662685,-2.28578961726445,
3.67752755953711));
#25603=CARTESIAN_POINT('Ctrl Pts',(-0.742636832700648,-4.32914134750355,
0.0870535403315232));
#25604=CARTESIAN_POINT('Ctrl Pts',(-0.623918622738608,-2.43178284203752,
-3.58266316233067));
#25605=CARTESIAN_POINT('Ctrl Pts',(-0.505200412776569,1.67916740539267,
-3.99117024821242));
#25606=CARTESIAN_POINT('Ctrl Pts',(-0.38648220281453,4.2616131179203,-0.766613826329018));
#25607=CARTESIAN_POINT('Ctrl Pts',(-0.267763992852492,2.96481787101653,
3.15577219032842));
#25608=CARTESIAN_POINT('Ctrl Pts',(-0.149045782890452,-1.03077771375419,
4.20553687778111));
#25609=CARTESIAN_POINT('Ctrl Pts',(-0.0303275729284135,-4.08808185427113,
1.42710541948671));
#25610=CARTESIAN_POINT('Ctrl Pts',(0.0883906370336247,-3.42410625029169,
-2.65038478569859));
#25611=CARTESIAN_POINT('Ctrl Pts',(0.207108846995665,0.356748537234746,
-4.31529530933053));
#25612=CARTESIAN_POINT('Ctrl Pts',(0.325827056957703,3.81286395974495,-2.05209930315938));
#25613=CARTESIAN_POINT('Ctrl Pts',(0.444545266919742,3.79822367634993,2.07907191553442));
#25614=CARTESIAN_POINT('Ctrl Pts',(0.56326347688178,0.326154374722222,4.31771542014972));
#25615=CARTESIAN_POINT('Ctrl Pts',(0.68198168684382,-3.44280518289795,2.62604942797354));
#25616=CARTESIAN_POINT('Ctrl Pts',(0.800699896805859,-4.0778643813607,-1.45604437184413));
#25617=CARTESIAN_POINT('Ctrl Pts',(0.919418106767897,-1.00094454806639,
-4.21273701258996));
#25618=CARTESIAN_POINT('Ctrl Pts',(1.03813631672994,2.98711033703512,-3.13467940305337));
#25619=CARTESIAN_POINT('Ctrl Pts',(1.15685452669198,4.25607260412292,0.796799293413037));
#25620=CARTESIAN_POINT('Ctrl Pts',(1.27557273665401,1.6508373043784,4.0029713114163));
#25621=CARTESIAN_POINT('Ctrl Pts',(1.39429094661605,-2.45711434039823,3.56533760585987));
#25622=CARTESIAN_POINT('Ctrl Pts',(1.51300915657809,-4.32841560712957,-0.117734691175787));
#25623=CARTESIAN_POINT('Ctrl Pts',(1.63172736654013,-2.25966726165839,-3.69363601240545));
#25624=CARTESIAN_POINT('Ctrl Pts',(1.75044557650217,1.86600027228884,-3.90731187766823));
#25625=CARTESIAN_POINT('Ctrl Pts',(1.86916378646421,4.29309393613648,-0.564258434635544));
#25626=CARTESIAN_POINT('Ctrl Pts',(1.98788199642625,2.8122904307839,3.29242549778585));
#25627=CARTESIAN_POINT('Ctrl Pts',(2.10660020638829,-1.22847145817667,4.1520959769729));
#25628=CARTESIAN_POINT('Ctrl Pts',(2.22531841635032,-4.15098617964756,1.23221623992068));
#25629=CARTESIAN_POINT('Ctrl Pts',(2.34403662631236,-3.29496090592035,-2.80931944677098));
#25630=CARTESIAN_POINT('Ctrl Pts',(2.4627548362744,0.560385740322455,-4.29360116307888));
#25631=CARTESIAN_POINT('Ctrl Pts',(2.58147304623644,3.90562711497251,-1.86952399405324));
#25632=CARTESIAN_POINT('Ctrl Pts',(2.70019125619848,3.69567277911633,2.25633460179288));
#25633=CARTESIAN_POINT('Ctrl Pts',(2.81890946616052,0.12163896896003,4.32830764696543));
#25634=CARTESIAN_POINT('Ctrl Pts',(2.93762767612256,-3.56311978445035,2.4603293534012));
#25635=CARTESIAN_POINT('Ctrl Pts',(3.05634588608459,-4.00445877432637,-1.64722586498323));
#25636=CARTESIAN_POINT('Ctrl Pts',(3.17506409604664,-0.800638039965777,
-4.25535214224499));
#25637=CARTESIAN_POINT('Ctrl Pts',(3.29378230600867,3.13198368884777,-2.98993667129265));
#25638=CARTESIAN_POINT('Ctrl Pts',(3.41250051597072,4.2136381726622,0.99714415980492));
#25639=CARTESIAN_POINT('Ctrl Pts',(3.53121872593275,1.45972210248142,4.07654933848181));
#25640=CARTESIAN_POINT('Ctrl Pts',(3.64993693589479,-2.62294287395784,3.44517253639104));
#25641=CARTESIAN_POINT('Ctrl Pts',(3.76865514585683,-4.31800786199842,-0.322259568157221));
#25642=CARTESIAN_POINT('Ctrl Pts',(3.88737335581887,-2.08249715066972,-3.79634676274463));
#25643=CARTESIAN_POINT('Ctrl Pts',(4.0060915657809,2.04865918151714,-3.81471344710645));
#25644=CARTESIAN_POINT('Ctrl Pts',(4.12480977574295,4.31497175877985,-0.360640882986961));
#25645=CARTESIAN_POINT('Ctrl Pts',(4.24352798570498,2.65347232629884,3.4217141521634));
#25646=CARTESIAN_POINT('Ctrl Pts',(4.36224619566703,-1.42341729953675,4.08936747149588));
#25647=CARTESIAN_POINT('Ctrl Pts',(4.48096440562906,-4.20460538280232,1.03457078078738));
#25648=CARTESIAN_POINT('Ctrl Pts',(4.59968261559111,-3.15844523714832,-2.96197008922851));
#25649=CARTESIAN_POINT('Ctrl Pts',(4.71840082555314,0.762769446080897,-4.2623028866652));
#25650=CARTESIAN_POINT('Ctrl Pts',(4.83711903551519,3.98965397873934,-1.68276684525171));
#25651=CARTESIAN_POINT('Ctrl Pts',(4.95583724547721,3.58485522621101,2.42855021209299));
#25652=CARTESIAN_POINT('Ctrl Pts',(5.07455545543927,-0.0831485246012159,
4.32921811051441));
#25653=CARTESIAN_POINT('Ctrl Pts',(5.19327366540129,-3.67546423113905,2.2891058977615));
#25654=CARTESIAN_POINT('Ctrl Pts',(5.31199187536334,-3.92209580450113,-1.83472276539637));
#25655=CARTESIAN_POINT('Ctrl Pts',(5.43071008532537,-0.598540626828496,
-4.28844869895689));
#25656=CARTESIAN_POINT('Ctrl Pts',(5.54942829528742,3.26985127140738,-2.83850590776641));
#25657=CARTESIAN_POINT('Ctrl Pts',(5.66814650524945,4.16177847603852,1.19525856697685));
#25658=CARTESIAN_POINT('Ctrl Pts',(5.78686471521149,1.2653417251431,4.14100874717272));
#25659=CARTESIAN_POINT('Ctrl Pts',(5.90558292517353,-2.78290428483595,3.31730114204168));
#25660=CARTESIAN_POINT('Ctrl Pts',(6.02430113513557,-4.29794139264672,-0.526063599694207));
#25661=CARTESIAN_POINT('Ctrl Pts',(6.1430193450976,-1.90066881155562,-3.89056566508378));
#25662=CARTESIAN_POINT('Ctrl Pts',(6.26173755505965,2.2267355529899,-3.71358208507633));
#25663=CARTESIAN_POINT('Ctrl Pts',(6.38045576502168,4.3271976485019,-0.156216632753608));
#25664=CARTESIAN_POINT('Ctrl Pts',(6.49917397498373,2.48871880940937,3.54334895448378));
#25665=CARTESIAN_POINT('Ctrl Pts',(6.61789218494576,-1.61517917375591,4.01749167543808));
#25666=CARTESIAN_POINT('Ctrl Pts',(6.7366103949078,-4.24881952576571,0.834611144798058));
#25667=CARTESIAN_POINT('Ctrl Pts',(6.85532860486984,-3.01486460868043,-3.10799525689398));
#25668=CARTESIAN_POINT('Ctrl Pts',(6.97404681483187,0.963446953064535,-4.22147048955455));
#25669=CARTESIAN_POINT('Ctrl Pts',(7.09276502479393,4.06475659578232,-1.4922456039785));
#25670=CARTESIAN_POINT('Ctrl Pts',(7.21148323475594,3.46601889957775,2.59533352641215));
#25671=CARTESIAN_POINT('Ctrl Pts',(7.33020144471801,-0.287750027609826,
4.32044477422867));
#25672=CARTESIAN_POINT('Ctrl Pts',(7.44891965468002,-3.77958722559195,2.1127620617787));
#25673=CARTESIAN_POINT('Ctrl Pts',(7.56763786464209,-3.83095970527152,-2.01811567114847));
#25674=CARTESIAN_POINT('Ctrl Pts',(7.6863560746041,-0.395104369707096,-4.31195265078218));
#25675=CARTESIAN_POINT('Ctrl Pts',(7.80507428456616,3.40040469598434,-2.68072583996889));
#25676=CARTESIAN_POINT('Ctrl Pts',(7.92379249452818,4.10060951647421,1.39069936325232));
#25677=CARTESIAN_POINT('Ctrl Pts',(8.04251070449023,1.06813097158531,4.19620535163489));
#25678=CARTESIAN_POINT('Ctrl Pts',(8.16122891445227,-2.93664076378281,3.18200945159473));
#25679=CARTESIAN_POINT('Ctrl Pts',(8.2799471244143,-4.26826108470218,-0.728690907289412));
#25680=CARTESIAN_POINT('Ctrl Pts',(8.39866533437635,-1.71458896654529,-3.97608196612575));
#25681=CARTESIAN_POINT('Ctrl Pts',(8.51738354433838,2.39983105705674,-3.60414400699182));
#25682=CARTESIAN_POINT('Ctrl Pts',(8.63610175430043,4.32974425785424,0.0485570502327038));
#25683=CARTESIAN_POINT('Ctrl Pts',(8.75481996426246,2.31839840857459,3.65705782626801));
#25684=CARTESIAN_POINT('Ctrl Pts',(8.8735381742245,-1.8033281388038,3.93662936397977));
#25685=CARTESIAN_POINT('Ctrl Pts',(8.99225638418654,-4.28352970825152,0.63278461112424));
#25686=CARTESIAN_POINT('Ctrl Pts',(9.11097459414858,-2.86454018845754,-3.24706831376562));
#25687=CARTESIAN_POINT('Ctrl Pts',(9.22969280411062,1.16196937633404,-4.17119530758405));
#25688=CARTESIAN_POINT('Ctrl Pts',(9.34841101407265,4.13076697301538,-1.29838643715753));
#25689=CARTESIAN_POINT('Ctrl Pts',(9.4671292240347,3.33942961793276,2.75631147594436));
#25690=CARTESIAN_POINT('Ctrl Pts',(9.58584743399673,-0.491707877746567,
4.30200726272179));
#25691=CARTESIAN_POINT('Ctrl Pts',(9.70456564395877,-3.8752558605702,1.93169229968585));
#25692=CARTESIAN_POINT('Ctrl Pts',(9.82328385392082,-3.73125433417492,-2.19699436031369));
#25693=CARTESIAN_POINT('Ctrl Pts',(9.94200206388284,-0.190784324443694,
-4.32581142296975));
#25694=CARTESIAN_POINT('Ctrl Pts',(10.0607202738449,3.52335193450366,-2.51694939781845));
#25695=CARTESIAN_POINT('Ctrl Pts',(10.1794384838069,4.03026811959114,1.58302937741427));
#25696=CARTESIAN_POINT('Ctrl Pts',(10.298156693769,0.868530972149402,4.24201568549269));
#25697=CARTESIAN_POINT('Ctrl Pts',(10.416874903731,-3.0838084257709,3.03960009190256));
#25698=CARTESIAN_POINT('Ctrl Pts',(10.5355931136931,-4.22903332848136,-0.929688244597408));
#25699=CARTESIAN_POINT('Ctrl Pts',(10.6543113236551,-1.5246738478374,-4.05270437896332));
#25700=CARTESIAN_POINT('Ctrl Pts',(10.7730295336171,2.56755850550722,-3.4866440091227));
#25701=CARTESIAN_POINT('Ctrl Pts',(10.8917477435791,4.32260589046018,0.253222118513249));
#25702=CARTESIAN_POINT('Ctrl Pts',(11.0104659535412,2.14289210452383,3.76258641813191));
#25703=CARTESIAN_POINT('Ctrl Pts',(11.1291841635032,-1.98744333417803,3.84696141376681));
#25704=CARTESIAN_POINT('Ctrl Pts',(11.2479023734653,-4.30865828887852,0.429542634896841));
#25705=CARTESIAN_POINT('Ctrl Pts',(11.3666205834273,-2.70780822925922,-3.37887817464105));
#25706=CARTESIAN_POINT('Ctrl Pts',(11.4853387933894,1.35789265155523,-4.11158979867935));
#25707=CARTESIAN_POINT('Ctrl Pts',(11.6040570033514,4.18753745528177,-1.10162297810297));
#25708=CARTESIAN_POINT('Ctrl Pts',(11.7227752133134,3.20537054221196,2.91112397752316));
#25709=CARTESIAN_POINT('Ctrl Pts',(11.8414934232755,-0.694565852527616,
4.27394681803398));
#25710=CARTESIAN_POINT('Ctrl Pts',(11.9602116332375,-3.96225613978983,1.7463016366203));
#25711=CARTESIAN_POINT('Ctrl Pts',(12.0789298431995,-3.62320271719853,-2.37095870806454));
#25712=CARTESIAN_POINT('Ctrl Pts',(12.1976480531616,0.0139624767857471,
-4.32999401654167));
#25713=CARTESIAN_POINT('Ctrl Pts',(12.3163662631236,3.63841797169183,-2.34754292234513));
#25714=CARTESIAN_POINT('Ctrl Pts',(12.4350844730857,3.9509116303975,1.77181839304862));
#25715=CARTESIAN_POINT('Ctrl Pts',(12.5538026830477,0.66698819766677,4.2783372847593));
#25716=CARTESIAN_POINT('Ctrl Pts',(12.6725208930098,-3.22407807181873,2.89039159814913));
#25717=CARTESIAN_POINT('Ctrl Pts',(12.7912391029718,-4.18034588454684,-1.12860598691075));
#25718=CARTESIAN_POINT('Ctrl Pts',(12.9099573129338,-1.33134823980997,-4.12026155727892));
#25719=CARTESIAN_POINT('Ctrl Pts',(13.0286755228959,2.72954266679506,-3.36134483293444));
#25720=CARTESIAN_POINT('Ctrl Pts',(13.1473937328579,4.30579861047257,0.457320600064824));
#25721=CARTESIAN_POINT('Ctrl Pts',(13.2661119428199,1.96259229413334,3.85969899730394));
#25722=CARTESIAN_POINT('Ctrl Pts',(13.384830152782,-2.16711257252377,3.74868779246955));
#25723=CARTESIAN_POINT('Ctrl Pts',(13.503548362744,-4.32414972403095,0.225340989528843));
#25724=CARTESIAN_POINT('Ctrl Pts',(13.6222665727061,-2.54501805154884,-3.50313219206192));
#25725=CARTESIAN_POINT('Ctrl Pts',(13.7409847826681,1.55077612259861,-4.04278312443387));
#25726=CARTESIAN_POINT('Ctrl Pts',(13.8597029926301,4.23494563063579,-0.902403280807197));
#25727=CARTESIAN_POINT('Ctrl Pts',(13.9784212025922,3.0641328417704,3.05943980887305));
#25728=CARTESIAN_POINT('Ctrl Pts',(14.0971394125542,-0.895853643967219,
4.23629754868133));
#25729=CARTESIAN_POINT('Ctrl Pts',(14.2158576225162,-4.04042492235024,1.55705926385799));
#25730=CARTESIAN_POINT('Ctrl Pts',(14.3345758324783,-3.50698671018115,-2.53972322927799));
#25731=CARTESIAN_POINT('Ctrl Pts',(14.4532940424403,0.218564245614825,-4.32429395921576));
#25732=CARTESIAN_POINT('Ctrl Pts',(14.5720122524024,3.74556186860945,-2.17326028708754));
#25733=CARTESIAN_POINT('Ctrl Pts',(14.6907304623644,3.86230569986296,1.95735778972818));
#25734=CARTESIAN_POINT('Ctrl Pts',(14.8094486723264,0.464738727873276,4.30372617863017));
#25735=CARTESIAN_POINT('Ctrl Pts',(14.9281668822885,-3.35864660907939,2.73735654780123));
#25736=CARTESIAN_POINT('Ctrl Pts',(15.0468850922505,-4.11928555052006,-1.33042058350709));
#25737=CARTESIAN_POINT('Ctrl Pts',(15.1260305655586,-2.13452904287985,-3.22024104752762));
#25738=CARTESIAN_POINT('Ctrl Pts',(15.1656033022126,-0.961289160296659,
-3.53893126683851));
#25739=CARTESIAN_POINT('Ctrl Pts',(-5.646,2.04569608541839,-2.86913603522103));
#25740=CARTESIAN_POINT('Ctrl Pts',(-5.60642726334599,2.99688291874876,-2.19093912940735));
#25741=CARTESIAN_POINT('Ctrl Pts',(-5.52728179003796,4.15588292084424,0.17368053733326));
#25742=CARTESIAN_POINT('Ctrl Pts',(-5.40856358007592,2.11478894550069,3.58630724545133));
#25743=CARTESIAN_POINT('Ctrl Pts',(-5.28984537011388,-1.85304107076213,
3.72388412481386));
#25744=CARTESIAN_POINT('Ctrl Pts',(-5.17112716015185,-4.13320183070728,
0.476987007469099));
#25745=CARTESIAN_POINT('Ctrl Pts',(-5.0524089501898,-2.65148029460583,-3.20684990304941));
#25746=CARTESIAN_POINT('Ctrl Pts',(-4.93369074022778,1.24406479104381,-3.9701278679622));
#25747=CARTESIAN_POINT('Ctrl Pts',(-4.81497253026572,4.0070387833704,-1.12025498671569));
#25748=CARTESIAN_POINT('Ctrl Pts',(-4.69625432030369,3.12257273473017,2.74975698427391));
#25749=CARTESIAN_POINT('Ctrl Pts',(-4.57753611034165,-0.604329863247786,
4.116523575551));
#25750=CARTESIAN_POINT('Ctrl Pts',(-4.45881790037961,-3.78110708392794,
1.73623086576801));
#25751=CARTESIAN_POINT('Ctrl Pts',(-4.34009969041758,-3.51604601315693,
-2.22456780215962));
#25752=CARTESIAN_POINT('Ctrl Pts',(-4.22138148045554,-0.0504100535793502,
-4.16036696958348));
#25753=CARTESIAN_POINT('Ctrl Pts',(-4.10266327049349,3.46111018837926,-2.30910306912985));
#25754=CARTESIAN_POINT('Ctrl Pts',(-3.98394506053146,3.82206891947539,1.64408864020745));
#25755=CARTESIAN_POINT('Ctrl Pts',(-3.86522685056942,0.703892139470341,
4.1007027146119));
#25756=CARTESIAN_POINT('Ctrl Pts',(-3.74650864060738,-3.05501983726778,
2.82455091812984));
#25757=CARTESIAN_POINT('Ctrl Pts',(-3.62779043064534,-4.03302306811295,
-1.02272090561931));
#25758=CARTESIAN_POINT('Ctrl Pts',(-3.5090722206833,-1.33986509473402,-3.93903455379817));
#25759=CARTESIAN_POINT('Ctrl Pts',(-3.39035401072126,2.57293885887897,-3.26974286547831));
#25760=CARTESIAN_POINT('Ctrl Pts',(-3.27163580075922,4.14366027205377,0.375915015385937));
#25761=CARTESIAN_POINT('Ctrl Pts',(-3.15291759079718,1.94251026639215,3.67938666679367));
#25762=CARTESIAN_POINT('Ctrl Pts',(-3.03419938083515,-2.0268587551866,3.63360373818345));
#25763=CARTESIAN_POINT('Ctrl Pts',(-2.9154811708731,-4.15122841486805,0.280241221310659));
#25764=CARTESIAN_POINT('Ctrl Pts',(-2.79676296091107,-2.4968375762945,-3.32821793059103));
#25765=CARTESIAN_POINT('Ctrl Pts',(-2.67804475094903,1.43036271770746,-3.90708267059147));
#25766=CARTESIAN_POINT('Ctrl Pts',(-2.55932654098699,4.05553922750062,-0.929426740059659));
#25767=CARTESIAN_POINT('Ctrl Pts',(-2.44060833102495,2.9890587402779,2.89426334951592));
#25768=CARTESIAN_POINT('Ctrl Pts',(-2.32189012106291,-0.798287948035305,
4.08337713718073));
#25769=CARTESIAN_POINT('Ctrl Pts',(-2.20317191110087,-3.858972872516,1.55549376734164));
#25770=CARTESIAN_POINT('Ctrl Pts',(-2.08445370113884,-3.40693028880043,
-2.38831708493618));
#25771=CARTESIAN_POINT('Ctrl Pts',(-1.96573549117679,0.14635662574293,-4.15810199844688));
#25772=CARTESIAN_POINT('Ctrl Pts',(-1.84701728121476,3.56641872576227,-2.14286956292151));
#25773=CARTESIAN_POINT('Ctrl Pts',(-1.72829907125272,3.74005811760244,1.82296400626149));
#25774=CARTESIAN_POINT('Ctrl Pts',(-1.60958086129068,0.509215159922919,
4.12939855331646));
#25775=CARTESIAN_POINT('Ctrl Pts',(-1.49086265132864,-3.18515375632809,
2.67694378718369));
#25776=CARTESIAN_POINT('Ctrl Pts',(-1.3721444413666,-3.98015603094717,-1.21226666229469));
#25777=CARTESIAN_POINT('Ctrl Pts',(-1.25342623140456,-1.15212076721019,
-3.99798076895909));
#25778=CARTESIAN_POINT('Ctrl Pts',(-1.13470802144252,2.72466151947467,-3.14443191936036));
#25779=CARTESIAN_POINT('Ctrl Pts',(-1.01598981148048,4.12125185197025,0.571415491416797));
#25780=CARTESIAN_POINT('Ctrl Pts',(-0.897271601518446,1.76636861191941,
3.76711752113286));
#25781=CARTESIAN_POINT('Ctrl Pts',(-0.778553391556407,-2.19639626337378,
3.53370569592844));
#25782=CARTESIAN_POINT('Ctrl Pts',(-0.659835181594368,-4.15983597416688,
0.083649024063062));
#25783=CARTESIAN_POINT('Ctrl Pts',(-0.541116971632329,-2.33667994081619,
-3.44255128435104));
#25784=CARTESIAN_POINT('Ctrl Pts',(-0.422398761670289,1.61349801702105,
-3.83508235117171));
#25785=CARTESIAN_POINT('Ctrl Pts',(-0.303680551708251,4.09494865907512,
-0.736632860208229));
#25786=CARTESIAN_POINT('Ctrl Pts',(-0.184962341746212,2.84886887415203,
3.0323552940062));
#25787=CARTESIAN_POINT('Ctrl Pts',(-0.0662441317841732,-0.990465746173143,
4.04106546554956));
#25788=CARTESIAN_POINT('Ctrl Pts',(0.0524740781778656,-3.92820390873641,
1.37129374773886));
#25789=CARTESIAN_POINT('Ctrl Pts',(0.171192288139904,-3.29019526413636,
-2.54673273333783));
#25790=CARTESIAN_POINT('Ctrl Pts',(0.289910498101944,0.342796707198351,
-4.1465314310558));
#25791=CARTESIAN_POINT('Ctrl Pts',(0.408628708063982,3.66374931913409,-1.97184518097748));
#25792=CARTESIAN_POINT('Ctrl Pts',(0.52734691802602,3.64968159238416,1.99776294024389));
#25793=CARTESIAN_POINT('Ctrl Pts',(0.64606512798806,0.313399030476065,4.14885689544678));
#25794=CARTESIAN_POINT('Ctrl Pts',(0.764783337950098,-3.30816291321273,
2.52334909016639));
#25795=CARTESIAN_POINT('Ctrl Pts',(0.883501547912138,-3.91838602385669,
-1.399100946767));
#25796=CARTESIAN_POINT('Ctrl Pts',(1.00221975787418,-0.961799304980866,
-4.04798401530169));
#25797=CARTESIAN_POINT('Ctrl Pts',(1.12093796783622,2.87028951964572,-3.01208740985575));
#25798=CARTESIAN_POINT('Ctrl Pts',(1.23965617779825,4.0896248253724,0.765637824886821));
#25799=CARTESIAN_POINT('Ctrl Pts',(1.35837438776029,1.586275858193,3.84642189481521));
#25800=CARTESIAN_POINT('Ctrl Pts',(1.47709259772233,-2.36102076725307,3.42590330099951));
#25801=CARTESIAN_POINT('Ctrl Pts',(1.59581080768437,-4.15913861626764,-0.11313028715101));
#25802=CARTESIAN_POINT('Ctrl Pts',(1.71452901764641,-2.17129550877666,-3.54918417453448));
#25803=CARTESIAN_POINT('Ctrl Pts',(1.83324722760845,1.7930241674711,-3.7545035392265));
#25804=CARTESIAN_POINT('Ctrl Pts',(1.95196543757049,4.12519831590081,-0.54219124457039));
#25805=CARTESIAN_POINT('Ctrl Pts',(2.07068364753253,2.70230652333086,3.16366432245317));
#25806=CARTESIAN_POINT('Ctrl Pts',(2.18940185749457,-1.18042802365586,3.98971454770484));
#25807=CARTESIAN_POINT('Ctrl Pts',(2.3081200674566,-3.98864815267002,1.18402635333924));
#25808=CARTESIAN_POINT('Ctrl Pts',(2.42683827741864,-3.16610057507709,-2.69945172946213));
#25809=CARTESIAN_POINT('Ctrl Pts',(2.54555648738068,0.538470004761492,-4.12568570605805));
#25810=CARTESIAN_POINT('Ctrl Pts',(2.66427469734272,3.75288466474145,-1.79641008245562));
#25811=CARTESIAN_POINT('Ctrl Pts',(2.78299290730476,3.55114128675486,2.16809318358432));
#25812=CARTESIAN_POINT('Ctrl Pts',(2.9017111172668,0.116881875255089,4.15903487824236));
#25813=CARTESIAN_POINT('Ctrl Pts',(3.02042932722884,-3.42377221482258,2.36411004655206));
#25814=CARTESIAN_POINT('Ctrl Pts',(3.13914753719088,-3.8478511855745,-1.58280565606543));
#25815=CARTESIAN_POINT('Ctrl Pts',(3.25786574715292,-0.769326444574681,
-4.08893253953619));
#25816=CARTESIAN_POINT('Ctrl Pts',(3.37658395711495,3.0094971204592,-2.87300532076558));
#25817=CARTESIAN_POINT('Ctrl Pts',(3.495302167077,4.04884993253241,0.958147543456581));
#25818=CARTESIAN_POINT('Ctrl Pts',(3.61402037703903,1.40263484759868,3.9171224100737));
#25819=CARTESIAN_POINT('Ctrl Pts',(3.73273858700107,-2.52036402820767,3.31043768352714));
#25820=CARTESIAN_POINT('Ctrl Pts',(3.8514567969631,-4.14913790039093,-0.309656543187913));
#25821=CARTESIAN_POINT('Ctrl Pts',(3.97017500692515,-2.00105422024427,-3.6478780816856));
#25822=CARTESIAN_POINT('Ctrl Pts',(4.08889321688719,1.96853959665618,-3.66552647618271));
#25823=CARTESIAN_POINT('Ctrl Pts',(4.20761142684923,4.14622053401822,-0.346536829911929));
#25824=CARTESIAN_POINT('Ctrl Pts',(4.32632963681127,2.54969952546351,3.28789671690745));
#25825=CARTESIAN_POINT('Ctrl Pts',(4.4450478467733,-1.3677498639029,3.92943924765267));
#25826=CARTESIAN_POINT('Ctrl Pts',(4.56376605673535,-4.04017039975903,0.994110472789965));
#25827=CARTESIAN_POINT('Ctrl Pts',(4.68248426669738,-3.03492380250006,-2.84613246427821));
#25828=CARTESIAN_POINT('Ctrl Pts',(4.80120247665942,0.732938827149255,-4.09561145213467));
#25829=CARTESIAN_POINT('Ctrl Pts',(4.91992068662146,3.83362538042524,-1.61695668889399));
#25830=CARTESIAN_POINT('Ctrl Pts',(5.0386388965835,3.44465762033206,2.33357373354433));
#25831=CARTESIAN_POINT('Ctrl Pts',(5.15735710654553,-0.0798967268727354,
4.15990973510661));
#25832=CARTESIAN_POINT('Ctrl Pts',(5.27607531650758,-3.5317230608034,2.19958284976698));
#25833=CARTESIAN_POINT('Ctrl Pts',(5.39479352646961,-3.76870929176318,-1.76296987080819));
#25834=CARTESIAN_POINT('Ctrl Pts',(5.51351173643166,-0.575132718389392,
-4.12073474606626));
#25835=CARTESIAN_POINT('Ctrl Pts',(5.63222994639369,3.14197293576922,-2.72749675748542));
#25836=CARTESIAN_POINT('Ctrl Pts',(5.75094815635573,3.99901838065921,1.14851403228232));
#25837=CARTESIAN_POINT('Ctrl Pts',(5.86966636631777,1.21585635703487,3.97906092065169));
#25838=CARTESIAN_POINT('Ctrl Pts',(5.98838457627981,-2.67406961969476,3.18756712246586));
#25839=CARTESIAN_POINT('Ctrl Pts',(6.10710278624185,-4.12985619661107,-0.505490144822725));
#25840=CARTESIAN_POINT('Ctrl Pts',(6.22582099620389,-1.82633687898537,-3.73841224260482));
#25841=CARTESIAN_POINT('Ctrl Pts',(6.34453920616593,2.13965170336266,-3.56835019014346));
#25842=CARTESIAN_POINT('Ctrl Pts',(6.46325741612797,4.15796828993553,-0.15010726528171));
#25843=CARTESIAN_POINT('Ctrl Pts',(6.58197562609,2.39138923910093,3.40477458847308));
#25844=CARTESIAN_POINT('Ctrl Pts',(6.70069383605204,-1.55201225656202,3.86037439203516));
#25845=CARTESIAN_POINT('Ctrl Pts',(6.81941204601408,-4.08265540260426,0.801970918915297));
#25846=CARTESIAN_POINT('Ctrl Pts',(6.93813025597612,-2.89695836881454,-2.98644683538066));
#25847=CARTESIAN_POINT('Ctrl Pts',(7.05684846593816,0.925768177301577,-4.05637594079931));
#25848=CARTESIAN_POINT('Ctrl Pts',(7.1755666759002,3.90579086153378,-1.43388641013115));
#25849=CARTESIAN_POINT('Ctrl Pts',(7.29428488586224,3.33046878081729,2.49383443540284));
#25850=CARTESIAN_POINT('Ctrl Pts',(7.41300309582428,-0.276496612222895,
4.15147950911829));
#25851=CARTESIAN_POINT('Ctrl Pts',(7.53172130578631,-3.63177398159695,2.03013552202684));
#25852=CARTESIAN_POINT('Ctrl Pts',(7.65043951574835,-3.68113737075413,-1.93919059115831));
#25853=CARTESIAN_POINT('Ctrl Pts',(7.76915772571038,-0.379652508136737,
-4.14331949821216));
#25854=CARTESIAN_POINT('Ctrl Pts',(7.88787593567244,3.26742063740621,-2.57588720045187));
#25855=CARTESIAN_POINT('Ctrl Pts',(8.00659414563445,3.940241635325,1.33631147059774));
#25856=CARTESIAN_POINT('Ctrl Pts',(8.12531235559652,1.02635818146356,4.03209887955918));
#25857=CARTESIAN_POINT('Ctrl Pts',(8.24403056555854,-2.82179372577729,3.0575664604982));
#25858=CARTESIAN_POINT('Ctrl Pts',(8.36274877552059,-4.10133663515502,-0.700193042192699));
#25859=CARTESIAN_POINT('Ctrl Pts',(8.48146698548262,-1.64753430101277,-3.82058414619887));
#25860=CARTESIAN_POINT('Ctrl Pts',(8.60018519544467,2.305977735937,-3.46319204962163));
#25861=CARTESIAN_POINT('Ctrl Pts',(8.7189034054067,4.16041530571664,0.0466580663793381));
#25862=CARTESIAN_POINT('Ctrl Pts',(8.83762161536874,2.22772978017945,3.5140364991988));
#25863=CARTESIAN_POINT('Ctrl Pts',(8.95633982533078,-1.73280303479793,3.78267446838806));
#25864=CARTESIAN_POINT('Ctrl Pts',(9.07505803529282,-4.11600812874189,0.608037478557221));
#25865=CARTESIAN_POINT('Ctrl Pts',(9.19377624525485,-2.75251288162813,-3.12008098094757));
#25866=CARTESIAN_POINT('Ctrl Pts',(9.31249445521691,1.11652672540754,-4.00806693589946));
#25867=CARTESIAN_POINT('Ctrl Pts',(9.43121266517893,3.96921968490559,-1.24760874642564));
#25868=CARTESIAN_POINT('Ctrl Pts',(9.54993087514098,3.20883019120772,2.64851681044191));
#25869=CARTESIAN_POINT('Ctrl Pts',(9.66864908510301,-0.472478016872994,
4.1337630574056));
#25870=CARTESIAN_POINT('Ctrl Pts',(9.78736729506506,-3.72370117857135,1.85614709112886));
#25871=CARTESIAN_POINT('Ctrl Pts',(9.90608550502709,-3.58533130756231,-2.11107363827349));
#25872=CARTESIAN_POINT('Ctrl Pts',(10.0248037149891,-0.183323073196887,
-4.15663627733209));
#25873=CARTESIAN_POINT('Ctrl Pts',(10.1435219249512,3.3855596180177,-2.41851577709298));
#25874=CARTESIAN_POINT('Ctrl Pts',(10.2622401349132,3.87265117113374,1.52111978421037));
#25875=CARTESIAN_POINT('Ctrl Pts',(10.3809583448753,0.834564199366861,4.07611764898101));
#25876=CARTESIAN_POINT('Ctrl Pts',(10.4996765548373,-2.96320591018775,2.92072648925374));
#25877=CARTESIAN_POINT('Ctrl Pts',(10.6183947647993,-4.0636430099267,-0.893329714648016));
#25878=CARTESIAN_POINT('Ctrl Pts',(10.7371129747614,-1.46504644039007,-3.89420998646693));
#25879=CARTESIAN_POINT('Ctrl Pts',(10.8558311847234,2.46714564844276,-3.35028727732022));
#25880=CARTESIAN_POINT('Ctrl Pts',(10.9745493946854,4.1535561077605,0.243319031071492));
#25881=CARTESIAN_POINT('Ctrl Pts',(11.0932676046475,2.05908722991844,3.61543804687332));
#25882=CARTESIAN_POINT('Ctrl Pts',(11.2119858146095,-1.90971779724849,3.69651327957846));
#25883=CARTESIAN_POINT('Ctrl Pts',(11.3307040245716,-4.14015397321339,0.412743951202418));
#25884=CARTESIAN_POINT('Ctrl Pts',(11.4494222345336,-2.60191044344467,-3.24673598179103));
#25885=CARTESIAN_POINT('Ctrl Pts',(11.5681404444956,1.30478777373567,-3.9507924973221));
#25886=CARTESIAN_POINT('Ctrl Pts',(11.6868586544577,4.02376996992659,-1.05854037242841));
#25887=CARTESIAN_POINT('Ctrl Pts',(11.8055768644197,3.0800139384955,2.79727485773682));
#25888=CARTESIAN_POINT('Ctrl Pts',(11.9242950743818,-0.66740256042652,4.10680000910255));
#25889=CARTESIAN_POINT('Ctrl Pts',(12.0430132843438,-3.80729902447422,1.67800674236445));
#25890=CARTESIAN_POINT('Ctrl Pts',(12.1617314943058,-3.48150540600691,-2.27823453552944));
#25891=CARTESIAN_POINT('Ctrl Pts',(12.2804497042679,0.0134164280071953,
-4.16065529676554));
#25892=CARTESIAN_POINT('Ctrl Pts',(12.3991679142299,3.49612561771096,-2.25573450146264));
#25893=CARTESIAN_POINT('Ctrl Pts',(12.5178861241919,3.79639817959729,1.70252558174023));
#25894=CARTESIAN_POINT('Ctrl Pts',(12.636604334154,0.640903420859428,4.11101877212304));
#25895=CARTESIAN_POINT('Ctrl Pts',(12.755322544116,-3.09798984835828,2.77735328654585));
#25896=CARTESIAN_POINT('Ctrl Pts',(12.8740407540781,-4.01685964932199,-1.08446812154071));
#25897=CARTESIAN_POINT('Ctrl Pts',(12.9927589640401,-1.2792814688989,-3.95912511815523));
#25898=CARTESIAN_POINT('Ctrl Pts',(13.1114771740022,2.62279488400284,-3.22988833933176));
#25899=CARTESIAN_POINT('Ctrl Pts',(13.2301953839642,4.1374061319782,0.439435567280381));
#25900=CARTESIAN_POINT('Ctrl Pts',(13.3489135939262,1.88583863921803,3.70875271783386));
#25901=CARTESIAN_POINT('Ctrl Pts',(13.4676318038883,-2.08236047650701,3.60208297288041));
#25902=CARTESIAN_POINT('Ctrl Pts',(13.5863500138503,-4.15503956461956,0.216528285738942));
#25903=CARTESIAN_POINT('Ctrl Pts',(13.7050682238123,-2.44548671339688,-3.36613063539831));
#25904=CARTESIAN_POINT('Ctrl Pts',(13.8237864337744,1.49012789947011,-3.88467673536986));
#25905=CARTESIAN_POINT('Ctrl Pts',(13.9425046437364,4.06932409197459,-0.867111819500367));
#25906=CARTESIAN_POINT('Ctrl Pts',(14.0612228536985,2.9442998048962,2.93979030855331));
#25907=CARTESIAN_POINT('Ctrl Pts',(14.1799410636605,-0.860818327845137,
4.07062313879903));
#25908=CARTESIAN_POINT('Ctrl Pts',(14.2986592736225,-3.88241075856883,1.49616531773476));
#25909=CARTESIAN_POINT('Ctrl Pts',(14.4173774835846,-3.36983440985343,-2.44039896264189));
#25910=CARTESIAN_POINT('Ctrl Pts',(14.5360956935466,0.210016568782032,-4.155178159011));
#25911=CARTESIAN_POINT('Ctrl Pts',(14.6548139035087,3.59907929859906,-2.08826776438434));
#25912=CARTESIAN_POINT('Ctrl Pts',(14.7735321134707,3.7112574766783,1.88080884739934));
#25913=CARTESIAN_POINT('Ctrl Pts',(14.8922503234327,0.446563584695773,4.13541474942909));
#25914=CARTESIAN_POINT('Ctrl Pts',(15.0109685333948,-3.22729563843389,2.6303031773798));
#25915=CARTESIAN_POINT('Ctrl Pts',(15.1296867433568,-3.95818728136483,-1.27839009166015));
#25916=CARTESIAN_POINT('Ctrl Pts',(15.2088322166648,-2.05105123342669,-3.09430288357736));
#25917=CARTESIAN_POINT('Ctrl Pts',(15.2484049533188,-0.923694772147997,
-3.40052966909663));
#25918=CARTESIAN_POINT('Ctrl Pts',(15.,-1.03647793659398,-3.81573446232228));
#25919=CARTESIAN_POINT('Ctrl Pts',(14.960427263346,-2.30148466178617,-3.47211737542815));
#25920=CARTESIAN_POINT('Ctrl Pts',(14.920854526692,-3.37148337530834,-2.45329947131456));
#25921=CARTESIAN_POINT('Ctrl Pts',(14.881281790038,-3.76979380899274,-1.21289970995026));
#25922=CARTESIAN_POINT('Ctrl Pts',(14.8689078082356,-3.89434132515796,-0.825039648387669));
#25923=CARTESIAN_POINT('Ctrl Pts',(14.8565338264332,-3.95321467832305,-0.415514473039758));
#25924=CARTESIAN_POINT('Ctrl Pts',(14.8441598446308,-3.95012252210193,-0.00484157028959653));
#25925=CARTESIAN_POINT('Origin',(15.4,4.91674827952517,-1.16214730382437));
#25926=CARTESIAN_POINT('',(20.4,4.68474025750198,-1.25527236874723));
#25927=CARTESIAN_POINT('',(20.4,4.91674827952517,-1.16214730382437));
#25928=CARTESIAN_POINT('',(15.4,4.68474025750198,-1.25527236874723));
#25929=CARTESIAN_POINT('',(15.4,4.68474025750198,-1.25527236874723));
#25930=CARTESIAN_POINT('',(15.4,4.91674827952517,-1.16214730382437));
#25931=CARTESIAN_POINT('Origin',(15.4,4.78133284013089,-1.28115427325748));
#25932=CARTESIAN_POINT('',(15.4,4.68474025750198,-1.25527236874723));
#25933=CARTESIAN_POINT('Origin',(15.4,4.68474025750198,-1.25527236874723));
#25934=CARTESIAN_POINT('',(20.4,4.68474025750198,-1.25527236874723));
#25935=CARTESIAN_POINT('Origin',(20.4,4.78133284013089,-1.28115427325748));
#25936=CARTESIAN_POINT('Origin',(15.4,4.44842828911141,-2.39509618943234));
#25937=CARTESIAN_POINT('',(20.4,4.20022320835453,-2.425));
#25938=CARTESIAN_POINT('',(20.4,4.44842828911141,-2.39509618943234));
#25939=CARTESIAN_POINT('',(15.4,4.20022320835453,-2.425));
#25940=CARTESIAN_POINT('',(15.4,4.20022320835453,-2.425));
#25941=CARTESIAN_POINT('',(15.4,4.44842828911141,-2.39509618943234));
#25942=CARTESIAN_POINT('Origin',(15.4,4.28682574873297,-2.475));
#25943=CARTESIAN_POINT('',(15.4,4.20022320835453,-2.425));
#25944=CARTESIAN_POINT('Origin',(15.4,4.20022320835453,-2.425));
#25945=CARTESIAN_POINT('',(20.4,4.20022320835453,-2.425));
#25946=CARTESIAN_POINT('Origin',(20.4,4.28682574873297,-2.475));
#25947=CARTESIAN_POINT('Origin',(15.4,3.67695526217005,-3.46482322781408));
#25948=CARTESIAN_POINT('',(20.4,3.42946788875475,-3.42946788875476));
#25949=CARTESIAN_POINT('',(20.4,3.67695526217005,-3.46482322781408));
#25950=CARTESIAN_POINT('',(15.4,3.42946788875475,-3.42946788875476));
#25951=CARTESIAN_POINT('',(15.4,3.42946788875475,-3.42946788875476));
#25952=CARTESIAN_POINT('',(15.4,3.67695526217005,-3.46482322781408));
#25953=CARTESIAN_POINT('Origin',(15.4,3.50017856687341,-3.50017856687341));
#25954=CARTESIAN_POINT('',(15.4,3.42946788875475,-3.42946788875476));
#25955=CARTESIAN_POINT('Origin',(15.4,3.42946788875475,-3.42946788875476));
#25956=CARTESIAN_POINT('',(20.4,3.42946788875475,-3.42946788875476));
#25957=CARTESIAN_POINT('Origin',(20.4,3.50017856687341,-3.50017856687341));
#25958=CARTESIAN_POINT('Origin',(15.4,2.65490381056766,-4.29842828911142));
#25959=CARTESIAN_POINT('',(20.4,2.425,-4.20022320835453));
#25960=CARTESIAN_POINT('',(20.4,2.65490381056766,-4.29842828911142));
#25961=CARTESIAN_POINT('',(15.4,2.425,-4.20022320835453));
#25962=CARTESIAN_POINT('',(15.4,2.425,-4.20022320835453));
#25963=CARTESIAN_POINT('',(15.4,2.65490381056766,-4.29842828911142));
#25964=CARTESIAN_POINT('Origin',(15.4,2.475,-4.28682574873297));
#25965=CARTESIAN_POINT('',(15.4,2.425,-4.20022320835453));
#25966=CARTESIAN_POINT('Origin',(15.4,2.425,-4.20022320835453));
#25967=CARTESIAN_POINT('',(20.4,2.425,-4.20022320835453));
#25968=CARTESIAN_POINT('Origin',(20.4,2.475,-4.28682574873297));
#25969=CARTESIAN_POINT('Origin',(15.4,1.45192505171109,-4.83910256599442));
#25970=CARTESIAN_POINT('',(20.4,1.25527236874722,-4.68474025750198));
#25971=CARTESIAN_POINT('',(20.4,1.45192505171109,-4.83910256599442));
#25972=CARTESIAN_POINT('',(15.4,1.25527236874722,-4.68474025750198));
#25973=CARTESIAN_POINT('',(15.4,1.25527236874722,-4.68474025750198));
#25974=CARTESIAN_POINT('',(15.4,1.45192505171109,-4.83910256599442));
#25975=CARTESIAN_POINT('Origin',(15.4,1.28115427325748,-4.78133284013089));
#25976=CARTESIAN_POINT('',(15.4,1.25527236874722,-4.68474025750198));
#25977=CARTESIAN_POINT('Origin',(15.4,1.25527236874722,-4.68474025750198));
#25978=CARTESIAN_POINT('',(20.4,1.25527236874722,-4.68474025750198));
#25979=CARTESIAN_POINT('Origin',(20.4,1.28115427325748,-4.78133284013089));
#25980=CARTESIAN_POINT('Origin',(15.4,0.149999999999999,-5.05));
#25981=CARTESIAN_POINT('',(20.4,-8.90930546379699E-16,-4.85));
#25982=CARTESIAN_POINT('',(20.4,0.149999999999999,-5.05));
#25983=CARTESIAN_POINT('',(15.4,-8.90930546379699E-16,-4.85));
#25984=CARTESIAN_POINT('',(15.4,-8.90930546379699E-16,-4.85));
#25985=CARTESIAN_POINT('',(15.4,0.149999999999999,-5.05));
#25986=CARTESIAN_POINT('Origin',(15.4,-9.0930024836691E-16,-4.95));
#25987=CARTESIAN_POINT('',(15.4,-8.90930546379699E-16,-4.85));
#25988=CARTESIAN_POINT('Origin',(15.4,-8.90930546379699E-16,-4.85));
#25989=CARTESIAN_POINT('',(20.4,-8.90930546379699E-16,-4.85));
#25990=CARTESIAN_POINT('Origin',(20.4,-9.0930024836691E-16,-4.95));
#25991=CARTESIAN_POINT('Origin',(15.4,-1.16214730382437,-4.91674827952517));
#25992=CARTESIAN_POINT('',(20.4,-1.25527236874723,-4.68474025750198));
#25993=CARTESIAN_POINT('',(20.4,-1.16214730382437,-4.91674827952517));
#25994=CARTESIAN_POINT('',(15.4,-1.25527236874723,-4.68474025750198));
#25995=CARTESIAN_POINT('',(15.4,-1.25527236874723,-4.68474025750198));
#25996=CARTESIAN_POINT('',(15.4,-1.16214730382437,-4.91674827952517));
#25997=CARTESIAN_POINT('Origin',(15.4,-1.28115427325748,-4.78133284013089));
#25998=CARTESIAN_POINT('',(15.4,-1.25527236874723,-4.68474025750198));
#25999=CARTESIAN_POINT('Origin',(15.4,-1.25527236874723,-4.68474025750198));
#26000=CARTESIAN_POINT('',(20.4,-1.25527236874723,-4.68474025750198));
#26001=CARTESIAN_POINT('Origin',(20.4,-1.28115427325748,-4.78133284013089));
#26002=CARTESIAN_POINT('Origin',(15.4,-2.39509618943234,-4.44842828911141));
#26003=CARTESIAN_POINT('',(20.4,-2.425,-4.20022320835453));
#26004=CARTESIAN_POINT('',(20.4,-2.39509618943234,-4.44842828911141));
#26005=CARTESIAN_POINT('',(15.4,-2.425,-4.20022320835453));
#26006=CARTESIAN_POINT('',(15.4,-2.425,-4.20022320835453));
#26007=CARTESIAN_POINT('',(15.4,-2.39509618943234,-4.44842828911141));
#26008=CARTESIAN_POINT('Origin',(15.4,-2.475,-4.28682574873297));
#26009=CARTESIAN_POINT('',(15.4,-2.425,-4.20022320835453));
#26010=CARTESIAN_POINT('Origin',(15.4,-2.425,-4.20022320835453));
#26011=CARTESIAN_POINT('',(20.4,-2.425,-4.20022320835453));
#26012=CARTESIAN_POINT('Origin',(20.4,-2.475,-4.28682574873297));
#26013=CARTESIAN_POINT('Origin',(15.4,-3.46482322781408,-3.67695526217005));
#26014=CARTESIAN_POINT('',(20.4,-3.42946788875476,-3.42946788875475));
#26015=CARTESIAN_POINT('',(20.4,-3.46482322781408,-3.67695526217005));
#26016=CARTESIAN_POINT('',(15.4,-3.42946788875476,-3.42946788875475));
#26017=CARTESIAN_POINT('',(15.4,-3.42946788875476,-3.42946788875475));
#26018=CARTESIAN_POINT('',(15.4,-3.46482322781408,-3.67695526217005));
#26019=CARTESIAN_POINT('Origin',(15.4,-3.50017856687341,-3.50017856687341));
#26020=CARTESIAN_POINT('',(15.4,-3.42946788875476,-3.42946788875475));
#26021=CARTESIAN_POINT('Origin',(15.4,-3.42946788875476,-3.42946788875475));
#26022=CARTESIAN_POINT('',(20.4,-3.42946788875476,-3.42946788875475));
#26023=CARTESIAN_POINT('Origin',(20.4,-3.50017856687341,-3.50017856687341));
#26024=CARTESIAN_POINT('Origin',(15.4,-4.29842828911142,-2.65490381056766));
#26025=CARTESIAN_POINT('',(20.4,-4.20022320835453,-2.425));
#26026=CARTESIAN_POINT('',(20.4,-4.29842828911142,-2.65490381056766));
#26027=CARTESIAN_POINT('',(15.4,-4.20022320835453,-2.425));
#26028=CARTESIAN_POINT('',(15.4,-4.20022320835453,-2.425));
#26029=CARTESIAN_POINT('',(15.4,-4.29842828911142,-2.65490381056766));
#26030=CARTESIAN_POINT('Origin',(15.4,-4.28682574873297,-2.475));
#26031=CARTESIAN_POINT('',(15.4,-4.20022320835453,-2.425));
#26032=CARTESIAN_POINT('Origin',(15.4,-4.20022320835453,-2.425));
#26033=CARTESIAN_POINT('',(20.4,-4.20022320835453,-2.425));
#26034=CARTESIAN_POINT('Origin',(20.4,-4.28682574873297,-2.475));
#26035=CARTESIAN_POINT('Origin',(15.4,-4.83910256599442,-1.45192505171109));
#26036=CARTESIAN_POINT('',(20.4,-4.68474025750198,-1.25527236874722));
#26037=CARTESIAN_POINT('',(20.4,-4.83910256599442,-1.45192505171109));
#26038=CARTESIAN_POINT('',(15.4,-4.68474025750198,-1.25527236874722));
#26039=CARTESIAN_POINT('',(15.4,-4.68474025750198,-1.25527236874722));
#26040=CARTESIAN_POINT('',(15.4,-4.83910256599442,-1.45192505171109));
#26041=CARTESIAN_POINT('Origin',(15.4,-4.78133284013089,-1.28115427325748));
#26042=CARTESIAN_POINT('',(15.4,-4.68474025750198,-1.25527236874722));
#26043=CARTESIAN_POINT('Origin',(15.4,-4.68474025750198,-1.25527236874722));
#26044=CARTESIAN_POINT('',(20.4,-4.68474025750198,-1.25527236874722));
#26045=CARTESIAN_POINT('Origin',(20.4,-4.78133284013089,-1.28115427325748));
#26046=CARTESIAN_POINT('Origin',(15.4,-5.05,-0.149999999999999));
#26047=CARTESIAN_POINT('',(20.4,-4.85,5.93953697586466E-16));
#26048=CARTESIAN_POINT('',(20.4,-5.05,-0.149999999999999));
#26049=CARTESIAN_POINT('',(15.4,-4.85,5.93953697586466E-16));
#26050=CARTESIAN_POINT('',(15.4,-4.85,5.93953697586466E-16));
#26051=CARTESIAN_POINT('',(15.4,-5.05,-0.149999999999999));
#26052=CARTESIAN_POINT('Origin',(15.4,-4.95,6.0620016557794E-16));
#26053=CARTESIAN_POINT('',(15.4,-4.85,5.93953697586466E-16));
#26054=CARTESIAN_POINT('Origin',(15.4,-4.85,5.93953697586466E-16));
#26055=CARTESIAN_POINT('',(20.4,-4.85,5.93953697586466E-16));
#26056=CARTESIAN_POINT('Origin',(20.4,-4.95,6.0620016557794E-16));
#26057=CARTESIAN_POINT('Origin',(15.4,-4.91674827952517,1.16214730382437));
#26058=CARTESIAN_POINT('',(20.4,-4.68474025750198,1.25527236874723));
#26059=CARTESIAN_POINT('',(20.4,-4.91674827952517,1.16214730382437));
#26060=CARTESIAN_POINT('',(15.4,-4.68474025750198,1.25527236874723));
#26061=CARTESIAN_POINT('',(15.4,-4.68474025750198,1.25527236874723));
#26062=CARTESIAN_POINT('',(15.4,-4.91674827952517,1.16214730382437));
#26063=CARTESIAN_POINT('Origin',(15.4,-4.78133284013089,1.28115427325748));
#26064=CARTESIAN_POINT('',(15.4,-4.68474025750198,1.25527236874723));
#26065=CARTESIAN_POINT('Origin',(15.4,-4.68474025750198,1.25527236874723));
#26066=CARTESIAN_POINT('',(20.4,-4.68474025750198,1.25527236874723));
#26067=CARTESIAN_POINT('Origin',(20.4,-4.78133284013089,1.28115427325748));
#26068=CARTESIAN_POINT('Origin',(15.4,-4.44842828911141,2.39509618943234));
#26069=CARTESIAN_POINT('',(20.4,-4.20022320835453,2.425));
#26070=CARTESIAN_POINT('',(20.4,-4.44842828911141,2.39509618943234));
#26071=CARTESIAN_POINT('',(15.4,-4.20022320835453,2.425));
#26072=CARTESIAN_POINT('',(15.4,-4.20022320835453,2.425));
#26073=CARTESIAN_POINT('',(15.4,-4.44842828911141,2.39509618943234));
#26074=CARTESIAN_POINT('Origin',(15.4,-4.28682574873297,2.475));
#26075=CARTESIAN_POINT('',(15.4,-4.20022320835453,2.425));
#26076=CARTESIAN_POINT('Origin',(15.4,-4.20022320835453,2.425));
#26077=CARTESIAN_POINT('',(20.4,-4.20022320835453,2.425));
#26078=CARTESIAN_POINT('Origin',(20.4,-4.28682574873297,2.475));
#26079=CARTESIAN_POINT('Origin',(15.4,-3.67695526217005,3.46482322781408));
#26080=CARTESIAN_POINT('',(20.4,-3.42946788875476,3.42946788875476));
#26081=CARTESIAN_POINT('',(20.4,-3.67695526217005,3.46482322781408));
#26082=CARTESIAN_POINT('',(15.4,-3.42946788875476,3.42946788875476));
#26083=CARTESIAN_POINT('',(15.4,-3.42946788875476,3.42946788875476));
#26084=CARTESIAN_POINT('',(15.4,-3.67695526217005,3.46482322781408));
#26085=CARTESIAN_POINT('Origin',(15.4,-3.50017856687341,3.50017856687341));
#26086=CARTESIAN_POINT('',(15.4,-3.42946788875476,3.42946788875476));
#26087=CARTESIAN_POINT('Origin',(15.4,-3.42946788875476,3.42946788875476));
#26088=CARTESIAN_POINT('',(20.4,-3.42946788875476,3.42946788875476));
#26089=CARTESIAN_POINT('Origin',(20.4,-3.50017856687341,3.50017856687341));
#26090=CARTESIAN_POINT('Origin',(15.4,-2.65490381056766,4.29842828911142));
#26091=CARTESIAN_POINT('',(20.4,-2.425,4.20022320835453));
#26092=CARTESIAN_POINT('',(20.4,-2.65490381056766,4.29842828911142));
#26093=CARTESIAN_POINT('',(15.4,-2.425,4.20022320835453));
#26094=CARTESIAN_POINT('',(15.4,-2.425,4.20022320835453));
#26095=CARTESIAN_POINT('',(15.4,-2.65490381056766,4.29842828911142));
#26096=CARTESIAN_POINT('Origin',(15.4,-2.475,4.28682574873297));
#26097=CARTESIAN_POINT('',(15.4,-2.425,4.20022320835453));
#26098=CARTESIAN_POINT('Origin',(15.4,-2.425,4.20022320835453));
#26099=CARTESIAN_POINT('',(20.4,-2.425,4.20022320835453));
#26100=CARTESIAN_POINT('Origin',(20.4,-2.475,4.28682574873297));
#26101=CARTESIAN_POINT('Origin',(15.4,-1.45192505171109,4.83910256599442));
#26102=CARTESIAN_POINT('',(20.4,-1.25527236874722,4.68474025750198));
#26103=CARTESIAN_POINT('',(20.4,-1.45192505171109,4.83910256599442));
#26104=CARTESIAN_POINT('',(15.4,-1.25527236874722,4.68474025750198));
#26105=CARTESIAN_POINT('',(15.4,-1.25527236874722,4.68474025750198));
#26106=CARTESIAN_POINT('',(15.4,-1.45192505171109,4.83910256599442));
#26107=CARTESIAN_POINT('Origin',(15.4,-1.28115427325748,4.78133284013089));
#26108=CARTESIAN_POINT('',(15.4,-1.25527236874722,4.68474025750198));
#26109=CARTESIAN_POINT('Origin',(15.4,-1.25527236874722,4.68474025750198));
#26110=CARTESIAN_POINT('',(20.4,-1.25527236874722,4.68474025750198));
#26111=CARTESIAN_POINT('Origin',(20.4,-1.28115427325748,4.78133284013089));
#26112=CARTESIAN_POINT('Origin',(15.4,-0.15,5.05));
#26113=CARTESIAN_POINT('',(20.4,2.96976848793233E-16,4.85));
#26114=CARTESIAN_POINT('',(20.4,-0.15,5.05));
#26115=CARTESIAN_POINT('',(15.4,2.96976848793233E-16,4.85));
#26116=CARTESIAN_POINT('',(15.4,2.96976848793233E-16,4.85));
#26117=CARTESIAN_POINT('',(15.4,-0.15,5.05));
#26118=CARTESIAN_POINT('Origin',(15.4,3.0310008278897E-16,4.95));
#26119=CARTESIAN_POINT('',(15.4,2.96976848793233E-16,4.85));
#26120=CARTESIAN_POINT('Origin',(15.4,2.96976848793233E-16,4.85));
#26121=CARTESIAN_POINT('',(20.4,2.96976848793233E-16,4.85));
#26122=CARTESIAN_POINT('Origin',(20.4,3.0310008278897E-16,4.95));
#26123=CARTESIAN_POINT('Origin',(15.4,1.16214730382437,4.91674827952517));
#26124=CARTESIAN_POINT('',(20.4,1.25527236874723,4.68474025750198));
#26125=CARTESIAN_POINT('',(20.4,1.16214730382437,4.91674827952517));
#26126=CARTESIAN_POINT('',(15.4,1.25527236874723,4.68474025750198));
#26127=CARTESIAN_POINT('',(15.4,1.25527236874723,4.68474025750198));
#26128=CARTESIAN_POINT('',(15.4,1.16214730382437,4.91674827952517));
#26129=CARTESIAN_POINT('Origin',(15.4,1.28115427325748,4.78133284013089));
#26130=CARTESIAN_POINT('',(15.4,1.25527236874723,4.68474025750198));
#26131=CARTESIAN_POINT('Origin',(15.4,1.25527236874723,4.68474025750198));
#26132=CARTESIAN_POINT('',(20.4,1.25527236874723,4.68474025750198));
#26133=CARTESIAN_POINT('Origin',(20.4,1.28115427325748,4.78133284013089));
#26134=CARTESIAN_POINT('Origin',(15.4,2.39509618943233,4.44842828911142));
#26135=CARTESIAN_POINT('',(20.4,2.425,4.20022320835453));
#26136=CARTESIAN_POINT('',(20.4,2.39509618943233,4.44842828911142));
#26137=CARTESIAN_POINT('',(15.4,2.425,4.20022320835453));
#26138=CARTESIAN_POINT('',(15.4,2.425,4.20022320835453));
#26139=CARTESIAN_POINT('',(15.4,2.39509618943233,4.44842828911142));
#26140=CARTESIAN_POINT('Origin',(15.4,2.475,4.28682574873297));
#26141=CARTESIAN_POINT('',(15.4,2.425,4.20022320835453));
#26142=CARTESIAN_POINT('Origin',(15.4,2.425,4.20022320835453));
#26143=CARTESIAN_POINT('',(20.4,2.425,4.20022320835453));
#26144=CARTESIAN_POINT('Origin',(20.4,2.475,4.28682574873297));
#26145=CARTESIAN_POINT('Origin',(15.4,3.46482322781408,3.67695526217005));
#26146=CARTESIAN_POINT('',(20.4,3.42946788875476,3.42946788875476));
#26147=CARTESIAN_POINT('',(20.4,3.46482322781408,3.67695526217005));
#26148=CARTESIAN_POINT('',(15.4,3.42946788875476,3.42946788875476));
#26149=CARTESIAN_POINT('',(15.4,3.42946788875476,3.42946788875476));
#26150=CARTESIAN_POINT('',(15.4,3.46482322781408,3.67695526217005));
#26151=CARTESIAN_POINT('Origin',(15.4,3.50017856687341,3.50017856687341));
#26152=CARTESIAN_POINT('',(15.4,3.42946788875476,3.42946788875476));
#26153=CARTESIAN_POINT('Origin',(15.4,3.42946788875476,3.42946788875476));
#26154=CARTESIAN_POINT('',(20.4,3.42946788875476,3.42946788875476));
#26155=CARTESIAN_POINT('Origin',(20.4,3.50017856687341,3.50017856687341));
#26156=CARTESIAN_POINT('Origin',(15.4,4.29842828911142,2.65490381056767));
#26157=CARTESIAN_POINT('',(20.4,4.20022320835453,2.425));
#26158=CARTESIAN_POINT('',(20.4,4.29842828911142,2.65490381056767));
#26159=CARTESIAN_POINT('',(15.4,4.20022320835453,2.425));
#26160=CARTESIAN_POINT('',(15.4,4.20022320835453,2.425));
#26161=CARTESIAN_POINT('',(15.4,4.29842828911142,2.65490381056767));
#26162=CARTESIAN_POINT('Origin',(15.4,4.28682574873297,2.475));
#26163=CARTESIAN_POINT('',(15.4,4.20022320835453,2.425));
#26164=CARTESIAN_POINT('Origin',(15.4,4.20022320835453,2.425));
#26165=CARTESIAN_POINT('',(20.4,4.20022320835453,2.425));
#26166=CARTESIAN_POINT('Origin',(20.4,4.28682574873297,2.475));
#26167=CARTESIAN_POINT('Origin',(15.4,4.83910256599442,1.45192505171109));
#26168=CARTESIAN_POINT('',(20.4,4.68474025750198,1.25527236874723));
#26169=CARTESIAN_POINT('',(20.4,4.83910256599442,1.45192505171109));
#26170=CARTESIAN_POINT('',(15.4,4.68474025750198,1.25527236874723));
#26171=CARTESIAN_POINT('',(15.4,4.68474025750198,1.25527236874723));
#26172=CARTESIAN_POINT('',(15.4,4.83910256599442,1.45192505171109));
#26173=CARTESIAN_POINT('Origin',(15.4,4.78133284013089,1.28115427325748));
#26174=CARTESIAN_POINT('',(15.4,4.68474025750198,1.25527236874723));
#26175=CARTESIAN_POINT('Origin',(15.4,4.68474025750198,1.25527236874723));
#26176=CARTESIAN_POINT('',(20.4,4.68474025750198,1.25527236874723));
#26177=CARTESIAN_POINT('Origin',(20.4,4.78133284013089,1.28115427325748));
#26178=CARTESIAN_POINT('Origin',(15.4,5.05,0.15));
#26179=CARTESIAN_POINT('',(20.4,4.85,0.));
#26180=CARTESIAN_POINT('',(20.4,5.05,0.15));
#26181=CARTESIAN_POINT('',(15.4,4.85,0.));
#26182=CARTESIAN_POINT('',(15.4,4.85,0.));
#26183=CARTESIAN_POINT('',(15.4,5.05,0.15));
#26184=CARTESIAN_POINT('Origin',(15.4,4.95,0.));
#26185=CARTESIAN_POINT('',(15.4,4.85,0.));
#26186=CARTESIAN_POINT('Origin',(15.4,4.85,0.));
#26187=CARTESIAN_POINT('',(20.4,4.85,0.));
#26188=CARTESIAN_POINT('Origin',(20.4,4.95,0.));
#26189=CARTESIAN_POINT('Origin',(-6.,3.6,0.));
#26190=CARTESIAN_POINT('',(-6.,-3.6,-4.40872847693047E-16));
#26191=CARTESIAN_POINT('Origin',(-6.,0.,0.));
#26192=CARTESIAN_POINT('Origin',(-5.8,0.,0.));
#26193=CARTESIAN_POINT('',(-5.8,-3.8,-4.65365783675994E-16));
#26194=CARTESIAN_POINT('Origin',(4.7,0.,0.));
#26195=CARTESIAN_POINT('Origin',(20.75,0.,0.));
#26196=CARTESIAN_POINT('',(21.,-4.5,-5.51091059616309E-16));
#26197=CARTESIAN_POINT('Origin',(21.,0.,0.));
#26198=CARTESIAN_POINT('',(20.75,-4.75,-5.81707229594993E-16));
#26199=CARTESIAN_POINT('Origin',(21.,3.,0.));
#26200=CARTESIAN_POINT('',(21.,-3.,-3.67394039744206E-16));
#26201=CARTESIAN_POINT('Origin',(21.,0.,0.));
#26202=CARTESIAN_POINT('Origin',(20.65,0.,0.));
#26203=CARTESIAN_POINT('',(20.3,-3.,-3.67394039744206E-16));
#26204=CARTESIAN_POINT('',(20.65,-3.,-3.67394039744206E-16));
#26205=CARTESIAN_POINT('Origin',(20.3,0.,0.));
#26206=CARTESIAN_POINT('Origin',(20.3,0.,0.));
#26207=CARTESIAN_POINT('',(0.,0.,0.));
#26208=CARTESIAN_POINT('Origin',(7.84,0.,0.));
#26209=CARTESIAN_POINT('',(7.68,2.15,-2.63299061816681E-16));
#26210=CARTESIAN_POINT('',(7.68,-2.15,-2.63299061816681E-16));
#26211=CARTESIAN_POINT('Origin',(7.68,0.,0.));
#26212=CARTESIAN_POINT('Origin',(7.68,0.,0.));
#26213=CARTESIAN_POINT('',(8.,2.47,3.02487759389396E-16));
#26214=CARTESIAN_POINT('',(7.84,2.31,-2.82893410603039E-16));
#26215=CARTESIAN_POINT('Origin',(8.,0.,0.));
#26216=CARTESIAN_POINT('Origin',(4.,0.,0.));
#26217=CARTESIAN_POINT('',(3.32,-2.15,-2.63299061816681E-16));
#26218=CARTESIAN_POINT('',(4.,-2.15,-2.63299061816681E-16));
#26219=CARTESIAN_POINT('Origin',(3.32,0.,0.));
#26220=CARTESIAN_POINT('Origin',(8.,2.15,0.));
#26221=CARTESIAN_POINT('',(8.,-5.9,-7.22541611496939E-16));
#26222=CARTESIAN_POINT('Origin',(8.,0.,0.));
#26223=CARTESIAN_POINT('Origin',(3.95,6.34315468735702,-0.634180373472705));
#26224=CARTESIAN_POINT('',(7.6395955992633,6.25001191701594,-0.360574957917378));
#26225=CARTESIAN_POINT('',(7.4,6.43629745752619,-0.907785788741997));
#26226=CARTESIAN_POINT('Ctrl Pts',(7.6395955992633,6.25001191701594,-0.360574957917378));
#26227=CARTESIAN_POINT('Ctrl Pts',(7.53289072318166,6.34140579300765,-0.629043024168655));
#26228=CARTESIAN_POINT('Ctrl Pts',(7.4,6.43629745752619,-0.907785788741997));
#26229=CARTESIAN_POINT('',(0.6,6.43629745752619,-0.907785788741997));
#26230=CARTESIAN_POINT('',(3.95,6.43629745752619,-0.907785788741997));
#26231=CARTESIAN_POINT('',(0.6,6.25001191718784,-0.360574958203413));
#26232=CARTESIAN_POINT('',(0.6,6.2727384556044,-0.427333805613703));
#26233=CARTESIAN_POINT('',(3.95,6.25001191718784,-0.360574958203413));
#26234=CARTESIAN_POINT('Origin',(3.95,0.,0.));
#26235=CARTESIAN_POINT('',(0.6,6.43629745752619,0.907785788741997));
#26236=CARTESIAN_POINT('Origin',(0.6,0.,0.));
#26237=CARTESIAN_POINT('',(7.4,6.29734418894816,-1.61042111446691));
#26238=CARTESIAN_POINT('Origin',(7.4,0.,0.));
#26239=CARTESIAN_POINT('',(7.38278617788904,6.29375806765092,-1.62437969264548));
#26240=CARTESIAN_POINT('Ctrl Pts',(7.38278617788871,6.29375806765085,-1.62437969264574));
#26241=CARTESIAN_POINT('Ctrl Pts',(7.38853745459905,6.29495796151265,-1.61972967166525));
#26242=CARTESIAN_POINT('Ctrl Pts',(7.39427239342974,6.29615711204027,-1.61507445283177));
#26243=CARTESIAN_POINT('Ctrl Pts',(7.3999909815365,6.2973543093563,-1.61041566515606));
#26244=CARTESIAN_POINT('',(0.6,6.29375806765092,-1.62437969264548));
#26245=CARTESIAN_POINT('',(3.95,6.29375806765092,-1.62437969264548));
#26246=CARTESIAN_POINT('',(0.6,5.59896890467484,-3.30174911289217));
#26247=CARTESIAN_POINT('Origin',(0.6,0.,0.));
#26248=CARTESIAN_POINT('',(7.38278617788903,5.59896890467484,-3.30174911289217));
#26249=CARTESIAN_POINT('',(3.95,5.59896890467484,-3.30174911289217));
#26250=CARTESIAN_POINT('',(7.40000076486337,5.5916352232277,-3.31415213071781));
#26251=CARTESIAN_POINT('Ctrl Pts',(7.40000076486337,5.5916352232277,-3.31415213071781));
#26252=CARTESIAN_POINT('Ctrl Pts',(7.39427320375822,5.59408570519366,-3.31001880145165));
#26253=CARTESIAN_POINT('Ctrl Pts',(7.38853488546801,5.59653040730634,-3.3058839072742));
#26254=CARTESIAN_POINT('Ctrl Pts',(7.38278617788892,5.59896890467488,-3.30174911289203));
#26255=CARTESIAN_POINT('',(7.4,5.19305106503475,-3.90924809086626));
#26256=CARTESIAN_POINT('Origin',(7.4,0.,0.));
#26257=CARTESIAN_POINT('',(0.6,5.19305106503475,-3.90924809086626));
#26258=CARTESIAN_POINT('',(3.95,5.19305106503475,-3.90924809086626));
#26259=CARTESIAN_POINT('',(0.6,3.90924809086626,-5.19305106503475));
#26260=CARTESIAN_POINT('Origin',(0.6,0.,0.));
#26261=CARTESIAN_POINT('',(7.4,3.90924809086626,-5.19305106503475));
#26262=CARTESIAN_POINT('',(3.95,3.90924809086626,-5.19305106503475));
#26263=CARTESIAN_POINT('',(7.4,3.30174911289217,-5.59896890467484));
#26264=CARTESIAN_POINT('Origin',(7.4,0.,0.));
#26265=CARTESIAN_POINT('',(0.6,3.30174911289217,-5.59896890467484));
#26266=CARTESIAN_POINT('',(3.95,3.30174911289217,-5.59896890467484));
#26267=CARTESIAN_POINT('',(0.6,1.62437969264548,-6.29375806765092));
#26268=CARTESIAN_POINT('Origin',(0.6,0.,0.));
#26269=CARTESIAN_POINT('',(7.4,1.62437969264548,-6.29375806765092));
#26270=CARTESIAN_POINT('',(3.95,1.62437969264548,-6.29375806765092));
#26271=CARTESIAN_POINT('',(7.4,0.907785788741996,-6.43629745752619));
#26272=CARTESIAN_POINT('Origin',(7.4,0.,0.));
#26273=CARTESIAN_POINT('',(0.6,0.907785788741996,-6.43629745752619));
#26274=CARTESIAN_POINT('',(3.95,0.907785788741996,-6.43629745752619));
#26275=CARTESIAN_POINT('',(0.6,-0.907785788741998,-6.43629745752619));
#26276=CARTESIAN_POINT('Origin',(0.6,0.,0.));
#26277=CARTESIAN_POINT('',(7.4,-0.907785788741998,-6.43629745752619));
#26278=CARTESIAN_POINT('',(3.95,-0.907785788741998,-6.43629745752619));
#26279=CARTESIAN_POINT('',(7.4,-1.62437969264548,-6.29375806765091));
#26280=CARTESIAN_POINT('Origin',(7.4,0.,0.));
#26281=CARTESIAN_POINT('',(0.6,-1.62437969264548,-6.29375806765092));
#26282=CARTESIAN_POINT('',(3.95,-1.62437969264548,-6.29375806765092));
#26283=CARTESIAN_POINT('',(0.6,-3.30174911289217,-5.59896890467484));
#26284=CARTESIAN_POINT('Origin',(0.6,0.,0.));
#26285=CARTESIAN_POINT('',(7.4,-3.30174911289217,-5.59896890467484));
#26286=CARTESIAN_POINT('',(3.95,-3.30174911289217,-5.59896890467484));
#26287=CARTESIAN_POINT('',(7.4,-3.90924809086626,-5.19305106503474));
#26288=CARTESIAN_POINT('Origin',(7.4,0.,0.));
#26289=CARTESIAN_POINT('',(0.6,-3.90924809086626,-5.19305106503474));
#26290=CARTESIAN_POINT('',(3.95,-3.90924809086626,-5.19305106503474));
#26291=CARTESIAN_POINT('',(0.6,-5.19305106503474,-3.90924809086626));
#26292=CARTESIAN_POINT('Origin',(0.6,0.,0.));
#26293=CARTESIAN_POINT('',(7.4,-5.19305106503474,-3.90924809086626));
#26294=CARTESIAN_POINT('',(3.95,-5.19305106503474,-3.90924809086626));
#26295=CARTESIAN_POINT('',(7.4,-5.59896890467484,-3.30174911289217));
#26296=CARTESIAN_POINT('Origin',(7.4,0.,0.));
#26297=CARTESIAN_POINT('',(0.6,-5.59896890467484,-3.30174911289217));
#26298=CARTESIAN_POINT('',(3.95,-5.59896890467484,-3.30174911289217));
#26299=CARTESIAN_POINT('',(0.6,-6.29375806765092,-1.62437969264548));
#26300=CARTESIAN_POINT('Origin',(0.6,0.,0.));
#26301=CARTESIAN_POINT('',(7.4,-6.29375806765092,-1.62437969264547));
#26302=CARTESIAN_POINT('',(3.95,-6.29375806765092,-1.62437969264548));
#26303=CARTESIAN_POINT('',(7.4,-6.43629745752619,-0.907785788741997));
#26304=CARTESIAN_POINT('Origin',(7.4,0.,0.));
#26305=CARTESIAN_POINT('',(0.6,-6.43629745752619,-0.907785788741997));
#26306=CARTESIAN_POINT('',(3.95,-6.43629745752619,-0.907785788741997));
#26307=CARTESIAN_POINT('',(0.6,-6.5,-7.9602041944578E-16));
#26308=CARTESIAN_POINT('Origin',(0.6,0.,0.));
#26309=CARTESIAN_POINT('',(0.500000000000001,-6.5,-7.9602041944578E-16));
#26310=CARTESIAN_POINT('',(3.95,-6.5,-7.9602041944578E-16));
#26311=CARTESIAN_POINT('Origin',(0.5,0.,0.));
#26312=CARTESIAN_POINT('',(0.6,-6.43629745752619,0.907785788741998));
#26313=CARTESIAN_POINT('Origin',(0.6,0.,0.));
#26314=CARTESIAN_POINT('',(7.4,-6.43629745752619,0.907785788741998));
#26315=CARTESIAN_POINT('',(3.95,-6.43629745752619,0.907785788741998));
#26316=CARTESIAN_POINT('',(7.4,-6.29375806765092,1.62437969264548));
#26317=CARTESIAN_POINT('Origin',(7.4,0.,0.));
#26318=CARTESIAN_POINT('',(0.6,-6.29375806765092,1.62437969264548));
#26319=CARTESIAN_POINT('',(3.95,-6.29375806765092,1.62437969264548));
#26320=CARTESIAN_POINT('',(0.6,-5.59896890467484,3.30174911289217));
#26321=CARTESIAN_POINT('Origin',(0.6,0.,0.));
#26322=CARTESIAN_POINT('',(7.4,-5.59896890467484,3.30174911289217));
#26323=CARTESIAN_POINT('',(3.95,-5.59896890467484,3.30174911289217));
#26324=CARTESIAN_POINT('',(7.4,-5.19305106503475,3.90924809086626));
#26325=CARTESIAN_POINT('Origin',(7.4,0.,0.));
#26326=CARTESIAN_POINT('',(0.6,-5.19305106503475,3.90924809086626));
#26327=CARTESIAN_POINT('',(3.95,-5.19305106503475,3.90924809086626));
#26328=CARTESIAN_POINT('',(0.6,-3.90924809086626,5.19305106503475));
#26329=CARTESIAN_POINT('Origin',(0.6,0.,0.));
#26330=CARTESIAN_POINT('',(7.4,-3.90924809086626,5.19305106503475));
#26331=CARTESIAN_POINT('',(3.95,-3.90924809086626,5.19305106503475));
#26332=CARTESIAN_POINT('',(7.4,-3.30174911289217,5.59896890467484));
#26333=CARTESIAN_POINT('Origin',(7.4,0.,0.));
#26334=CARTESIAN_POINT('',(0.6,-3.30174911289217,5.59896890467484));
#26335=CARTESIAN_POINT('',(3.95,-3.30174911289217,5.59896890467484));
#26336=CARTESIAN_POINT('',(0.6,-1.62437969264548,6.29375806765092));
#26337=CARTESIAN_POINT('Origin',(0.6,0.,0.));
#26338=CARTESIAN_POINT('',(7.4,-1.62437969264548,6.29375806765092));
#26339=CARTESIAN_POINT('',(3.95,-1.62437969264548,6.29375806765092));
#26340=CARTESIAN_POINT('',(7.4,-0.907785788741997,6.43629745752619));
#26341=CARTESIAN_POINT('Origin',(7.4,0.,0.));
#26342=CARTESIAN_POINT('',(0.6,-0.907785788741997,6.43629745752619));
#26343=CARTESIAN_POINT('',(3.95,-0.907785788741997,6.43629745752619));
#26344=CARTESIAN_POINT('',(0.6,0.907785788741998,6.43629745752619));
#26345=CARTESIAN_POINT('Origin',(0.6,0.,0.));
#26346=CARTESIAN_POINT('',(7.4,0.907785788741998,6.43629745752619));
#26347=CARTESIAN_POINT('',(3.95,0.907785788741998,6.43629745752619));
#26348=CARTESIAN_POINT('',(7.4,1.62437969264548,6.29375806765092));
#26349=CARTESIAN_POINT('Origin',(7.4,0.,0.));
#26350=CARTESIAN_POINT('',(0.6,1.62437969264548,6.29375806765092));
#26351=CARTESIAN_POINT('',(3.95,1.62437969264548,6.29375806765092));
#26352=CARTESIAN_POINT('',(0.6,3.30174911289217,5.59896890467484));
#26353=CARTESIAN_POINT('Origin',(0.6,0.,0.));
#26354=CARTESIAN_POINT('',(7.4,3.30174911289217,5.59896890467484));
#26355=CARTESIAN_POINT('',(3.95,3.30174911289217,5.59896890467484));
#26356=CARTESIAN_POINT('',(7.4,3.90924809086626,5.19305106503475));
#26357=CARTESIAN_POINT('Origin',(7.4,0.,0.));
#26358=CARTESIAN_POINT('',(0.6,3.90924809086626,5.19305106503475));
#26359=CARTESIAN_POINT('',(3.95,3.90924809086626,5.19305106503475));
#26360=CARTESIAN_POINT('',(0.6,5.19305106503475,3.90924809086626));
#26361=CARTESIAN_POINT('Origin',(0.6,0.,0.));
#26362=CARTESIAN_POINT('',(7.4,5.19305106503475,3.90924809086626));
#26363=CARTESIAN_POINT('',(3.95,5.19305106503475,3.90924809086626));
#26364=CARTESIAN_POINT('',(7.4,5.59896890467484,3.30174911289217));
#26365=CARTESIAN_POINT('Origin',(7.4,0.,0.));
#26366=CARTESIAN_POINT('',(0.6,5.59896890467484,3.30174911289217));
#26367=CARTESIAN_POINT('',(3.95,5.59896890467484,3.30174911289217));
#26368=CARTESIAN_POINT('',(0.6,6.29375806765092,1.62437969264548));
#26369=CARTESIAN_POINT('Origin',(0.6,0.,0.));
#26370=CARTESIAN_POINT('',(7.4,6.29375806765092,1.62437969264548));
#26371=CARTESIAN_POINT('',(3.95,6.29375806765092,1.62437969264548));
#26372=CARTESIAN_POINT('',(7.4,6.43629745752619,0.907785788741997));
#26373=CARTESIAN_POINT('Origin',(7.4,0.,0.));
#26374=CARTESIAN_POINT('',(3.95,6.43629745752619,0.907785788741997));
#26375=CARTESIAN_POINT('Origin',(7.7,0.,0.));
#26376=CARTESIAN_POINT('',(7.75,-6.15,8.74596390859847E-17));
#26377=CARTESIAN_POINT('',(7.7,-6.2,-7.59281015471359E-16));
#26378=CARTESIAN_POINT('',(7.6395955992633,-6.25001191701594,-0.360574957917378));
#26379=CARTESIAN_POINT('Ctrl Pts',(7.75,-6.15,9.28077059647592E-16));
#26380=CARTESIAN_POINT('Ctrl Pts',(7.75,-6.15,-0.080715219171627));
#26381=CARTESIAN_POINT('Ctrl Pts',(7.73340207567264,-6.16485627699069,-0.16401583254945));
#26382=CARTESIAN_POINT('Ctrl Pts',(7.6858526263557,-6.20786999945922,-0.282558774022249));
#26383=CARTESIAN_POINT('Ctrl Pts',(7.66390188127962,-6.22779773364639,-0.323611089501759));
#26384=CARTESIAN_POINT('Ctrl Pts',(7.63959559912056,-6.2500119169745,-0.360574957848419));
#26385=CARTESIAN_POINT('Ctrl Pts',(7.4,-6.43629745752619,-0.907785788741997));
#26386=CARTESIAN_POINT('Ctrl Pts',(7.53289072319445,-6.34140579300535,-0.629043024174526));
#26387=CARTESIAN_POINT('Ctrl Pts',(7.6395955992633,-6.25001191701594,-0.360574957917378));
#26388=CARTESIAN_POINT('',(7.6395955992633,-5.91224415060338,-2.05864818917039));
#26389=CARTESIAN_POINT('Ctrl Pts',(7.6395955992633,-5.91224415060338,-2.05864818917039));
#26390=CARTESIAN_POINT('Ctrl Pts',(7.53289072318166,-6.09941936310245,-1.84559095978961));
#26391=CARTESIAN_POINT('Ctrl Pts',(7.4,-6.29375806765092,-1.62437969264548));
#26392=CARTESIAN_POINT('',(7.6395955992633,-5.63627202556194,-2.72490383628236));
#26393=CARTESIAN_POINT('Ctrl Pts',(7.63959559912056,-5.91224415053871,-2.05864818921824));
#26394=CARTESIAN_POINT('Ctrl Pts',(7.66390188127962,-5.87757546121802,-2.08429735070297));
#26395=CARTESIAN_POINT('Ctrl Pts',(7.6858526263557,-5.84345459447894,-2.11459873101868));
#26396=CARTESIAN_POINT('Ctrl Pts',(7.73340207567264,-5.75835067694767,-2.20765748941603));
#26397=CARTESIAN_POINT('Ctrl Pts',(7.75,-5.71274750206111,-2.27893197009047));
#26398=CARTESIAN_POINT('Ctrl Pts',(7.75,-5.65097074782772,-2.42807424800013));
#26399=CARTESIAN_POINT('Ctrl Pts',(7.73340207567264,-5.63281839342319,-2.5107192308165));
#26400=CARTESIAN_POINT('Ctrl Pts',(7.68585262635569,-5.62719347150353,-2.63669926711996));
#26401=CARTESIAN_POINT('Ctrl Pts',(7.66390188127962,-5.62989425625414,-2.68225267487168));
#26402=CARTESIAN_POINT('Ctrl Pts',(7.63959559912056,-5.63627202555004,-2.72490383620279));
#26403=CARTESIAN_POINT('Ctrl Pts',(7.4,-5.59896890467484,-3.30174911289217));
#26404=CARTESIAN_POINT('Ctrl Pts',(7.53289072319445,-5.61797067590973,-3.00791090999099));
#26405=CARTESIAN_POINT('Ctrl Pts',(7.6395955992633,-5.63627202556194,-2.72490383628236));
#26406=CARTESIAN_POINT('',(7.6395955992633,-4.67439080688814,-4.16446081114928));
#26407=CARTESIAN_POINT('Ctrl Pts',(7.6395955992633,-4.67439080688814,-4.16446081114928));
#26408=CARTESIAN_POINT('Ctrl Pts',(7.53289072318166,-4.92885162653911,-4.03925045044361));
#26409=CARTESIAN_POINT('Ctrl Pts',(7.4,-5.19305106503474,-3.90924809086626));
#26410=CARTESIAN_POINT('',(7.6395955992633,-4.16446081114928,-4.67439080688814));
#26411=CARTESIAN_POINT('Ctrl Pts',(7.63959559912056,-4.67439080681007,-4.16446081116873));
#26412=CARTESIAN_POINT('Ctrl Pts',(7.66390188127962,-4.63254560517343,-4.17489041346571));
#26413=CARTESIAN_POINT('Ctrl Pts',(7.6858526263557,-4.58942619853704,-4.18982774814726));
#26414=CARTESIAN_POINT('Ctrl Pts',(7.73340207567264,-4.47518838591824,-4.2432349710829));
#26415=CARTESIAN_POINT('Ctrl Pts',(7.75,-4.40578098311848,-4.29163242547605));
#26416=CARTESIAN_POINT('Ctrl Pts',(7.75,-4.29163242547605,-4.40578098311848));
#26417=CARTESIAN_POINT('Ctrl Pts',(7.73340207567264,-4.2432349710829,-4.47518838591824));
#26418=CARTESIAN_POINT('Ctrl Pts',(7.68585262635569,-4.18982774814726,-4.58942619853704));
#26419=CARTESIAN_POINT('Ctrl Pts',(7.66390188127962,-4.17489041346571,-4.63254560517343));
#26420=CARTESIAN_POINT('Ctrl Pts',(7.63959559912056,-4.16446081116873,-4.67439080681007));
#26421=CARTESIAN_POINT('Ctrl Pts',(7.4,-3.90924809086626,-5.19305106503474));
#26422=CARTESIAN_POINT('Ctrl Pts',(7.53289072319445,-4.03925045043784,-4.92885162654163));
#26423=CARTESIAN_POINT('Ctrl Pts',(7.6395955992633,-4.16446081114928,-4.67439080688814));
#26424=CARTESIAN_POINT('',(7.6395955992633,-2.72490383628237,-5.63627202556194));
#26425=CARTESIAN_POINT('Ctrl Pts',(7.6395955992633,-2.72490383628237,-5.63627202556194));
#26426=CARTESIAN_POINT('Ctrl Pts',(7.53289072318165,-3.00791090998646,-5.61797067591409));
#26427=CARTESIAN_POINT('Ctrl Pts',(7.4,-3.30174911289217,-5.59896890467484));
#26428=CARTESIAN_POINT('',(7.6395955992633,-2.0586481891704,-5.91224415060338));
#26429=CARTESIAN_POINT('Ctrl Pts',(7.63959559912056,-2.7249038362028,-5.63627202555004));
#26430=CARTESIAN_POINT('Ctrl Pts',(7.66390188127961,-2.68225267487168,-5.62989425625414));
#26431=CARTESIAN_POINT('Ctrl Pts',(7.6858526263557,-2.63669926711997,-5.62719347150352));
#26432=CARTESIAN_POINT('Ctrl Pts',(7.73340207567264,-2.51071923081651,-5.63281839342319));
#26433=CARTESIAN_POINT('Ctrl Pts',(7.75,-2.42807424800014,-5.65097074782771));
#26434=CARTESIAN_POINT('Ctrl Pts',(7.75,-2.27893197009048,-5.71274750206111));
#26435=CARTESIAN_POINT('Ctrl Pts',(7.73340207567264,-2.20765748941603,-5.75835067694767));
#26436=CARTESIAN_POINT('Ctrl Pts',(7.6858526263557,-2.11459873101869,-5.84345459447893));
#26437=CARTESIAN_POINT('Ctrl Pts',(7.66390188127962,-2.08429735070298,-5.87757546121802));
#26438=CARTESIAN_POINT('Ctrl Pts',(7.63959559912056,-2.05864818921825,-5.91224415053871));
#26439=CARTESIAN_POINT('Ctrl Pts',(7.4,-1.62437969264548,-6.29375806765091));
#26440=CARTESIAN_POINT('Ctrl Pts',(7.53289072319445,-1.84559095978331,-6.09941936310257));
#26441=CARTESIAN_POINT('Ctrl Pts',(7.6395955992633,-2.0586481891704,-5.91224415060338));
#26442=CARTESIAN_POINT('',(7.6395955992633,-0.360574957917379,-6.25001191701594));
#26443=CARTESIAN_POINT('Ctrl Pts',(7.6395955992633,-0.360574957917379,-6.25001191701594));
#26444=CARTESIAN_POINT('Ctrl Pts',(7.53289072318166,-0.629043024168655,
-6.34140579300765));
#26445=CARTESIAN_POINT('Ctrl Pts',(7.4,-0.907785788741998,-6.43629745752619));
#26446=CARTESIAN_POINT('',(7.6395955992633,0.360574957917378,-6.25001191701594));
#26447=CARTESIAN_POINT('Ctrl Pts',(7.63959559912056,-0.360574957848421,
-6.2500119169745));
#26448=CARTESIAN_POINT('Ctrl Pts',(7.66390188127962,-0.323611089501761,
-6.22779773364639));
#26449=CARTESIAN_POINT('Ctrl Pts',(7.68585262635569,-0.282558774022252,
-6.20786999945922));
#26450=CARTESIAN_POINT('Ctrl Pts',(7.73340207567264,-0.164015832549453,
-6.16485627699069));
#26451=CARTESIAN_POINT('Ctrl Pts',(7.75,-0.0807152191716292,-6.15));
#26452=CARTESIAN_POINT('Ctrl Pts',(7.75,0.0807152191716266,-6.15));
#26453=CARTESIAN_POINT('Ctrl Pts',(7.73340207567264,0.16401583254945,-6.16485627699069));
#26454=CARTESIAN_POINT('Ctrl Pts',(7.6858526263557,0.28255877402225,-6.20786999945922));
#26455=CARTESIAN_POINT('Ctrl Pts',(7.66390188127962,0.32361108950176,-6.22779773364639));
#26456=CARTESIAN_POINT('Ctrl Pts',(7.63959559912056,0.36057495784842,-6.2500119169745));
#26457=CARTESIAN_POINT('Ctrl Pts',(7.4,0.907785788741996,-6.43629745752619));
#26458=CARTESIAN_POINT('Ctrl Pts',(7.53289072319445,0.629043024174527,-6.34140579300535));
#26459=CARTESIAN_POINT('Ctrl Pts',(7.6395955992633,0.360574957917378,-6.25001191701594));
#26460=CARTESIAN_POINT('',(7.6395955992633,2.05864818917039,-5.91224415060338));
#26461=CARTESIAN_POINT('Ctrl Pts',(7.6395955992633,2.05864818917039,-5.91224415060338));
#26462=CARTESIAN_POINT('Ctrl Pts',(7.53289072318166,1.84559095978961,-6.09941936310245));
#26463=CARTESIAN_POINT('Ctrl Pts',(7.4,1.62437969264548,-6.29375806765092));
#26464=CARTESIAN_POINT('',(7.6395955992633,2.72490383628236,-5.63627202556194));
#26465=CARTESIAN_POINT('Ctrl Pts',(7.63959559912056,2.05864818921824,-5.91224415053871));
#26466=CARTESIAN_POINT('Ctrl Pts',(7.66390188127961,2.08429735070297,-5.87757546121802));
#26467=CARTESIAN_POINT('Ctrl Pts',(7.6858526263557,2.11459873101869,-5.84345459447894));
#26468=CARTESIAN_POINT('Ctrl Pts',(7.73340207567264,2.20765748941603,-5.75835067694767));
#26469=CARTESIAN_POINT('Ctrl Pts',(7.75,2.27893197009047,-5.71274750206111));
#26470=CARTESIAN_POINT('Ctrl Pts',(7.75,2.42807424800013,-5.65097074782771));
#26471=CARTESIAN_POINT('Ctrl Pts',(7.73340207567264,2.5107192308165,-5.63281839342319));
#26472=CARTESIAN_POINT('Ctrl Pts',(7.68585262635569,2.63669926711996,-5.62719347150352));
#26473=CARTESIAN_POINT('Ctrl Pts',(7.66390188127962,2.68225267487168,-5.62989425625414));
#26474=CARTESIAN_POINT('Ctrl Pts',(7.63959559912056,2.72490383620279,-5.63627202555004));
#26475=CARTESIAN_POINT('Ctrl Pts',(7.4,3.30174911289217,-5.59896890467484));
#26476=CARTESIAN_POINT('Ctrl Pts',(7.53289072319445,3.007910909991,-5.61797067590972));
#26477=CARTESIAN_POINT('Ctrl Pts',(7.6395955992633,2.72490383628236,-5.63627202556194));
#26478=CARTESIAN_POINT('',(7.6395955992633,4.16446081114928,-4.67439080688814));
#26479=CARTESIAN_POINT('Ctrl Pts',(7.6395955992633,4.16446081114928,-4.67439080688814));
#26480=CARTESIAN_POINT('Ctrl Pts',(7.53289072318166,4.03925045044361,-4.92885162653911));
#26481=CARTESIAN_POINT('Ctrl Pts',(7.4,3.90924809086626,-5.19305106503475));
#26482=CARTESIAN_POINT('',(7.6395955992633,4.67439080688814,-4.16446081114928));
#26483=CARTESIAN_POINT('Ctrl Pts',(7.63959559912056,4.16446081116873,-4.67439080681008));
#26484=CARTESIAN_POINT('Ctrl Pts',(7.66390188127962,4.17489041346571,-4.63254560517344));
#26485=CARTESIAN_POINT('Ctrl Pts',(7.68585262635569,4.18982774814726,-4.58942619853704));
#26486=CARTESIAN_POINT('Ctrl Pts',(7.73340207567264,4.24323497108289,-4.47518838591825));
#26487=CARTESIAN_POINT('Ctrl Pts',(7.75,4.29163242547605,-4.40578098311848));
#26488=CARTESIAN_POINT('Ctrl Pts',(7.75,4.40578098311848,-4.29163242547605));
#26489=CARTESIAN_POINT('Ctrl Pts',(7.73340207567264,4.47518838591824,-4.2432349710829));
#26490=CARTESIAN_POINT('Ctrl Pts',(7.6858526263557,4.58942619853704,-4.18982774814726));
#26491=CARTESIAN_POINT('Ctrl Pts',(7.66390188127962,4.63254560517343,-4.17489041346571));
#26492=CARTESIAN_POINT('Ctrl Pts',(7.63959559912056,4.67439080681008,-4.16446081116873));
#26493=CARTESIAN_POINT('Ctrl Pts',(7.4,5.19305106503475,-3.90924809086626));
#26494=CARTESIAN_POINT('Ctrl Pts',(7.53289072319445,4.92885162654163,-4.03925045043784));
#26495=CARTESIAN_POINT('Ctrl Pts',(7.6395955992633,4.67439080688814,-4.16446081114928));
#26496=CARTESIAN_POINT('Ctrl Pts',(7.40000051046853,6.29734425077455,-1.6104165295937));
#26497=CARTESIAN_POINT('Ctrl Pts',(7.47330660022597,6.21996344948776,-1.6170670263044));
#26498=CARTESIAN_POINT('Ctrl Pts',(7.6818261033525,5.99172758842293,-1.66250658304213));
#26499=CARTESIAN_POINT('Ctrl Pts',(7.97308777074854,5.61920950447284,-1.91938073772091));
#26500=CARTESIAN_POINT('Ctrl Pts',(7.98425119443302,5.38246983194813,-2.46771855869631));
#26501=CARTESIAN_POINT('Ctrl Pts',(7.81463329279646,5.37650527564507,-2.85267802239966));
#26502=CARTESIAN_POINT('Ctrl Pts',(7.62197014916225,5.45315318247101,-3.11162923149047));
#26503=CARTESIAN_POINT('Ctrl Pts',(7.47355913123751,5.54155404080058,-3.25437523675975));
#26504=CARTESIAN_POINT('Ctrl Pts',(7.399999514344,5.59163607462568,-3.31415314694812));
#26505=CARTESIAN_POINT('',(7.6395955992633,6.25001191701594,0.360574957917378));
#26506=CARTESIAN_POINT('Ctrl Pts',(7.63959559912056,6.2500119169745,-0.36057495784842));
#26507=CARTESIAN_POINT('Ctrl Pts',(7.66390188127962,6.22779773364639,-0.323611089501758));
#26508=CARTESIAN_POINT('Ctrl Pts',(7.6858526263557,6.20786999945922,-0.282558774022251));
#26509=CARTESIAN_POINT('Ctrl Pts',(7.73340207567264,6.16485627699069,-0.164015832549452));
#26510=CARTESIAN_POINT('Ctrl Pts',(7.75,6.15,-0.0807152191716278));
#26511=CARTESIAN_POINT('Ctrl Pts',(7.75,6.15,0.080715219171628));
#26512=CARTESIAN_POINT('Ctrl Pts',(7.73340207567264,6.16485627699069,0.164015832549452));
#26513=CARTESIAN_POINT('Ctrl Pts',(7.6858526263557,6.20786999945922,0.282558774022251));
#26514=CARTESIAN_POINT('Ctrl Pts',(7.66390188127961,6.22779773364639,0.32361108950176));
#26515=CARTESIAN_POINT('Ctrl Pts',(7.63959559912056,6.2500119169745,0.36057495784842));
#26516=CARTESIAN_POINT('Ctrl Pts',(7.4,6.43629745752619,0.907785788741997));
#26517=CARTESIAN_POINT('Ctrl Pts',(7.53289072319445,6.34140579300535,0.629043024174527));
#26518=CARTESIAN_POINT('Ctrl Pts',(7.6395955992633,6.25001191701594,0.360574957917378));
#26519=CARTESIAN_POINT('',(7.6395955992633,5.91224415060338,2.05864818917039));
#26520=CARTESIAN_POINT('Ctrl Pts',(7.6395955992633,5.91224415060338,2.05864818917039));
#26521=CARTESIAN_POINT('Ctrl Pts',(7.53289072318166,6.09941936310245,1.84559095978961));
#26522=CARTESIAN_POINT('Ctrl Pts',(7.4,6.29375806765092,1.62437969264548));
#26523=CARTESIAN_POINT('',(7.6395955992633,5.63627202556194,2.72490383628236));
#26524=CARTESIAN_POINT('Ctrl Pts',(7.63959559912056,5.91224415053871,2.05864818921824));
#26525=CARTESIAN_POINT('Ctrl Pts',(7.66390188127962,5.87757546121802,2.08429735070297));
#26526=CARTESIAN_POINT('Ctrl Pts',(7.6858526263557,5.84345459447894,2.11459873101869));
#26527=CARTESIAN_POINT('Ctrl Pts',(7.73340207567264,5.75835067694767,2.20765748941603));
#26528=CARTESIAN_POINT('Ctrl Pts',(7.75,5.71274750206111,2.27893197009047));
#26529=CARTESIAN_POINT('Ctrl Pts',(7.75,5.65097074782771,2.42807424800013));
#26530=CARTESIAN_POINT('Ctrl Pts',(7.73340207567264,5.63281839342319,2.5107192308165));
#26531=CARTESIAN_POINT('Ctrl Pts',(7.6858526263557,5.62719347150352,2.63669926711996));
#26532=CARTESIAN_POINT('Ctrl Pts',(7.66390188127962,5.62989425625414,2.68225267487168));
#26533=CARTESIAN_POINT('Ctrl Pts',(7.63959559912056,5.63627202555004,2.72490383620279));
#26534=CARTESIAN_POINT('Ctrl Pts',(7.4,5.59896890467484,3.30174911289217));
#26535=CARTESIAN_POINT('Ctrl Pts',(7.53289072319445,5.61797067590972,3.007910909991));
#26536=CARTESIAN_POINT('Ctrl Pts',(7.6395955992633,5.63627202556194,2.72490383628236));
#26537=CARTESIAN_POINT('',(7.6395955992633,4.67439080688814,4.16446081114928));
#26538=CARTESIAN_POINT('Ctrl Pts',(7.6395955992633,4.67439080688814,4.16446081114928));
#26539=CARTESIAN_POINT('Ctrl Pts',(7.53289072318166,4.92885162653911,4.03925045044362));
#26540=CARTESIAN_POINT('Ctrl Pts',(7.4,5.19305106503475,3.90924809086626));
#26541=CARTESIAN_POINT('',(7.6395955992633,4.16446081114928,4.67439080688814));
#26542=CARTESIAN_POINT('Ctrl Pts',(7.63959559912056,4.67439080681008,4.16446081116873));
#26543=CARTESIAN_POINT('Ctrl Pts',(7.66390188127962,4.63254560517343,4.17489041346571));
#26544=CARTESIAN_POINT('Ctrl Pts',(7.6858526263557,4.58942619853704,4.18982774814726));
#26545=CARTESIAN_POINT('Ctrl Pts',(7.73340207567264,4.47518838591824,4.2432349710829));
#26546=CARTESIAN_POINT('Ctrl Pts',(7.75,4.40578098311848,4.29163242547605));
#26547=CARTESIAN_POINT('Ctrl Pts',(7.75,4.29163242547605,4.40578098311848));
#26548=CARTESIAN_POINT('Ctrl Pts',(7.73340207567264,4.2432349710829,4.47518838591824));
#26549=CARTESIAN_POINT('Ctrl Pts',(7.6858526263557,4.18982774814726,4.58942619853704));
#26550=CARTESIAN_POINT('Ctrl Pts',(7.66390188127962,4.17489041346571,4.63254560517343));
#26551=CARTESIAN_POINT('Ctrl Pts',(7.63959559912056,4.16446081116873,4.67439080681008));
#26552=CARTESIAN_POINT('Ctrl Pts',(7.4,3.90924809086626,5.19305106503475));
#26553=CARTESIAN_POINT('Ctrl Pts',(7.53289072319445,4.03925045043784,4.92885162654164));
#26554=CARTESIAN_POINT('Ctrl Pts',(7.6395955992633,4.16446081114928,4.67439080688814));
#26555=CARTESIAN_POINT('',(7.6395955992633,2.72490383628236,5.63627202556194));
#26556=CARTESIAN_POINT('Ctrl Pts',(7.6395955992633,2.72490383628236,5.63627202556194));
#26557=CARTESIAN_POINT('Ctrl Pts',(7.53289072318166,3.00791090998645,5.61797067591409));
#26558=CARTESIAN_POINT('Ctrl Pts',(7.4,3.30174911289217,5.59896890467484));
#26559=CARTESIAN_POINT('',(7.6395955992633,2.05864818917039,5.91224415060338));
#26560=CARTESIAN_POINT('Ctrl Pts',(7.63959559912056,2.72490383620279,5.63627202555004));
#26561=CARTESIAN_POINT('Ctrl Pts',(7.66390188127962,2.68225267487168,5.62989425625414));
#26562=CARTESIAN_POINT('Ctrl Pts',(7.6858526263557,2.63669926711996,5.62719347150352));
#26563=CARTESIAN_POINT('Ctrl Pts',(7.73340207567264,2.5107192308165,5.63281839342319));
#26564=CARTESIAN_POINT('Ctrl Pts',(7.75,2.42807424800013,5.65097074782771));
#26565=CARTESIAN_POINT('Ctrl Pts',(7.75,2.27893197009047,5.71274750206111));
#26566=CARTESIAN_POINT('Ctrl Pts',(7.73340207567264,2.20765748941603,5.75835067694767));
#26567=CARTESIAN_POINT('Ctrl Pts',(7.6858526263557,2.11459873101869,5.84345459447894));
#26568=CARTESIAN_POINT('Ctrl Pts',(7.66390188127962,2.08429735070298,5.87757546121802));
#26569=CARTESIAN_POINT('Ctrl Pts',(7.63959559912056,2.05864818921824,5.9122441505387));
#26570=CARTESIAN_POINT('Ctrl Pts',(7.4,1.62437969264548,6.29375806765092));
#26571=CARTESIAN_POINT('Ctrl Pts',(7.53289072319445,1.8455909597833,6.09941936310257));
#26572=CARTESIAN_POINT('Ctrl Pts',(7.6395955992633,2.05864818917039,5.91224415060338));
#26573=CARTESIAN_POINT('',(7.6395955992633,0.360574957917379,6.25001191701594));
#26574=CARTESIAN_POINT('Ctrl Pts',(7.6395955992633,0.360574957917379,6.25001191701594));
#26575=CARTESIAN_POINT('Ctrl Pts',(7.53289072318166,0.629043024168653,6.34140579300765));
#26576=CARTESIAN_POINT('Ctrl Pts',(7.4,0.907785788741998,6.43629745752619));
#26577=CARTESIAN_POINT('',(7.6395955992633,-0.360574957917378,6.25001191701594));
#26578=CARTESIAN_POINT('Ctrl Pts',(7.63959559912056,0.36057495784842,6.2500119169745));
#26579=CARTESIAN_POINT('Ctrl Pts',(7.66390188127962,0.32361108950176,6.22779773364639));
#26580=CARTESIAN_POINT('Ctrl Pts',(7.6858526263557,0.282558774022251,6.20786999945922));
#26581=CARTESIAN_POINT('Ctrl Pts',(7.73340207567264,0.164015832549452,6.16485627699069));
#26582=CARTESIAN_POINT('Ctrl Pts',(7.75,0.0807152191716284,6.15));
#26583=CARTESIAN_POINT('Ctrl Pts',(7.75,-0.0807152191716275,6.15));
#26584=CARTESIAN_POINT('Ctrl Pts',(7.73340207567264,-0.16401583254945,6.16485627699069));
#26585=CARTESIAN_POINT('Ctrl Pts',(7.6858526263557,-0.282558774022249,6.20786999945922));
#26586=CARTESIAN_POINT('Ctrl Pts',(7.66390188127962,-0.323611089501759,
6.22779773364639));
#26587=CARTESIAN_POINT('Ctrl Pts',(7.63959559912056,-0.360574957848421,
6.2500119169745));
#26588=CARTESIAN_POINT('Ctrl Pts',(7.4,-0.907785788741997,6.43629745752619));
#26589=CARTESIAN_POINT('Ctrl Pts',(7.53289072319445,-0.629043024174527,
6.34140579300535));
#26590=CARTESIAN_POINT('Ctrl Pts',(7.6395955992633,-0.360574957917378,6.25001191701594));
#26591=CARTESIAN_POINT('',(7.6395955992633,-2.05864818917039,5.91224415060338));
#26592=CARTESIAN_POINT('Ctrl Pts',(7.6395955992633,-2.05864818917039,5.91224415060338));
#26593=CARTESIAN_POINT('Ctrl Pts',(7.53289072318166,-1.84559095978961,6.09941936310245));
#26594=CARTESIAN_POINT('Ctrl Pts',(7.4,-1.62437969264548,6.29375806765092));
#26595=CARTESIAN_POINT('',(7.6395955992633,-2.72490383628236,5.63627202556194));
#26596=CARTESIAN_POINT('Ctrl Pts',(7.63959559912056,-2.05864818921824,5.91224415053871));
#26597=CARTESIAN_POINT('Ctrl Pts',(7.66390188127962,-2.08429735070297,5.87757546121802));
#26598=CARTESIAN_POINT('Ctrl Pts',(7.6858526263557,-2.11459873101868,5.84345459447894));
#26599=CARTESIAN_POINT('Ctrl Pts',(7.73340207567264,-2.20765748941603,5.75835067694767));
#26600=CARTESIAN_POINT('Ctrl Pts',(7.75,-2.27893197009047,5.71274750206111));
#26601=CARTESIAN_POINT('Ctrl Pts',(7.75,-2.42807424800013,5.65097074782771));
#26602=CARTESIAN_POINT('Ctrl Pts',(7.73340207567264,-2.5107192308165,5.63281839342319));
#26603=CARTESIAN_POINT('Ctrl Pts',(7.6858526263557,-2.63669926711996,5.62719347150352));
#26604=CARTESIAN_POINT('Ctrl Pts',(7.66390188127962,-2.68225267487168,5.62989425625414));
#26605=CARTESIAN_POINT('Ctrl Pts',(7.63959559912056,-2.72490383620279,5.63627202555004));
#26606=CARTESIAN_POINT('Ctrl Pts',(7.4,-3.30174911289217,5.59896890467484));
#26607=CARTESIAN_POINT('Ctrl Pts',(7.53289072319445,-3.007910909991,5.61797067590973));
#26608=CARTESIAN_POINT('Ctrl Pts',(7.6395955992633,-2.72490383628236,5.63627202556194));
#26609=CARTESIAN_POINT('',(7.6395955992633,-4.16446081114928,4.67439080688814));
#26610=CARTESIAN_POINT('Ctrl Pts',(7.6395955992633,-4.16446081114928,4.67439080688814));
#26611=CARTESIAN_POINT('Ctrl Pts',(7.53289072318166,-4.03925045044361,4.92885162653911));
#26612=CARTESIAN_POINT('Ctrl Pts',(7.4,-3.90924809086626,5.19305106503475));
#26613=CARTESIAN_POINT('',(7.6395955992633,-4.67439080688814,4.16446081114928));
#26614=CARTESIAN_POINT('Ctrl Pts',(7.63959559912056,-4.16446081116873,4.67439080681008));
#26615=CARTESIAN_POINT('Ctrl Pts',(7.66390188127962,-4.17489041346571,4.63254560517343));
#26616=CARTESIAN_POINT('Ctrl Pts',(7.6858526263557,-4.18982774814726,4.58942619853704));
#26617=CARTESIAN_POINT('Ctrl Pts',(7.73340207567264,-4.2432349710829,4.47518838591824));
#26618=CARTESIAN_POINT('Ctrl Pts',(7.75,-4.29163242547605,4.40578098311848));
#26619=CARTESIAN_POINT('Ctrl Pts',(7.75,-4.40578098311848,4.29163242547605));
#26620=CARTESIAN_POINT('Ctrl Pts',(7.73340207567264,-4.47518838591824,4.2432349710829));
#26621=CARTESIAN_POINT('Ctrl Pts',(7.6858526263557,-4.58942619853704,4.18982774814726));
#26622=CARTESIAN_POINT('Ctrl Pts',(7.66390188127962,-4.63254560517344,4.17489041346571));
#26623=CARTESIAN_POINT('Ctrl Pts',(7.63959559912056,-4.67439080681008,4.16446081116873));
#26624=CARTESIAN_POINT('Ctrl Pts',(7.4,-5.19305106503475,3.90924809086626));
#26625=CARTESIAN_POINT('Ctrl Pts',(7.53289072319445,-4.92885162654164,4.03925045043784));
#26626=CARTESIAN_POINT('Ctrl Pts',(7.6395955992633,-4.67439080688814,4.16446081114927));
#26627=CARTESIAN_POINT('',(7.6395955992633,-5.63627202556194,2.72490383628236));
#26628=CARTESIAN_POINT('Ctrl Pts',(7.6395955992633,-5.63627202556194,2.72490383628236));
#26629=CARTESIAN_POINT('Ctrl Pts',(7.53289072318166,-5.61797067591409,3.00791090998645));
#26630=CARTESIAN_POINT('Ctrl Pts',(7.4,-5.59896890467484,3.30174911289217));
#26631=CARTESIAN_POINT('',(7.6395955992633,-5.91224415060338,2.05864818917039));
#26632=CARTESIAN_POINT('Ctrl Pts',(7.63959559912056,-5.63627202555004,2.72490383620279));
#26633=CARTESIAN_POINT('Ctrl Pts',(7.66390188127962,-5.62989425625414,2.68225267487168));
#26634=CARTESIAN_POINT('Ctrl Pts',(7.6858526263557,-5.62719347150352,2.63669926711996));
#26635=CARTESIAN_POINT('Ctrl Pts',(7.73340207567264,-5.63281839342319,2.5107192308165));
#26636=CARTESIAN_POINT('Ctrl Pts',(7.75,-5.65097074782771,2.42807424800013));
#26637=CARTESIAN_POINT('Ctrl Pts',(7.75,-5.71274750206111,2.27893197009047));
#26638=CARTESIAN_POINT('Ctrl Pts',(7.73340207567264,-5.75835067694767,2.20765748941603));
#26639=CARTESIAN_POINT('Ctrl Pts',(7.6858526263557,-5.84345459447894,2.11459873101869));
#26640=CARTESIAN_POINT('Ctrl Pts',(7.66390188127962,-5.87757546121802,2.08429735070297));
#26641=CARTESIAN_POINT('Ctrl Pts',(7.63959559912056,-5.91224415053871,2.05864818921824));
#26642=CARTESIAN_POINT('Ctrl Pts',(7.4,-6.29375806765092,1.62437969264548));
#26643=CARTESIAN_POINT('Ctrl Pts',(7.53289072319445,-6.09941936310258,1.8455909597833));
#26644=CARTESIAN_POINT('Ctrl Pts',(7.6395955992633,-5.91224415060338,2.05864818917039));
#26645=CARTESIAN_POINT('',(7.6395955992633,-6.25001191701594,0.360574957917379));
#26646=CARTESIAN_POINT('Ctrl Pts',(7.6395955992633,-6.25001191701594,0.360574957917379));
#26647=CARTESIAN_POINT('Ctrl Pts',(7.53289072318166,-6.34140579300764,0.629043024168652));
#26648=CARTESIAN_POINT('Ctrl Pts',(7.4,-6.43629745752619,0.907785788741998));
#26649=CARTESIAN_POINT('Ctrl Pts',(7.63959559912056,-6.2500119169745,0.360574957848422));
#26650=CARTESIAN_POINT('Ctrl Pts',(7.66390188127962,-6.22779773364639,0.32361108950176));
#26651=CARTESIAN_POINT('Ctrl Pts',(7.6858526263557,-6.20786999945922,0.282558774022252));
#26652=CARTESIAN_POINT('Ctrl Pts',(7.73340207567264,-6.16485627699069,0.164015832549452));
#26653=CARTESIAN_POINT('Ctrl Pts',(7.75,-6.15,0.0807152191716289));
#26654=CARTESIAN_POINT('Ctrl Pts',(7.75,-6.15,9.28077059647592E-16));
#26655=CARTESIAN_POINT('Origin',(3.95,6.34315468735702,0.634180373472705));
#26656=CARTESIAN_POINT('',(0.6,6.25001191718784,0.360574958203413));
#26657=CARTESIAN_POINT('',(3.95,6.25001191718784,0.360574958203413));
#26658=CARTESIAN_POINT('',(0.6,6.2727384556044,0.427333805613703));
#26659=CARTESIAN_POINT('Origin',(3.95,6.10300110926129,1.84151394080869));
#26660=CARTESIAN_POINT('',(0.6,5.91224415087166,2.05864818897191));
#26661=CARTESIAN_POINT('',(0.6,5.95878823942725,2.00566812596253));
#26662=CARTESIAN_POINT('',(3.95,5.91224415087166,2.05864818897191));
#26663=CARTESIAN_POINT('Origin',(3.95,5.61762046514307,3.01332647475229));
#26664=CARTESIAN_POINT('',(0.6,5.63627202561129,2.72490383661241));
#26665=CARTESIAN_POINT('',(3.95,5.63627202561129,2.72490383661241));
#26666=CARTESIAN_POINT('',(0.6,5.63172110443148,2.79527803907584));
#26667=CARTESIAN_POINT('Origin',(3.95,4.93372093612335,4.03685445096741));
#26668=CARTESIAN_POINT('',(0.6,4.67439080721195,4.16446081106857));
#26669=CARTESIAN_POINT('',(0.6,4.73766653034721,4.1333252667878));
#26670=CARTESIAN_POINT('',(3.95,4.67439080721195,4.16446081106857));
#26671=CARTESIAN_POINT('Origin',(3.95,4.03685445096741,4.93372093612335));
#26672=CARTESIAN_POINT('',(0.6,4.16446081106857,4.67439080721195));
#26673=CARTESIAN_POINT('',(3.95,4.16446081106857,4.67439080721195));
#26674=CARTESIAN_POINT('',(0.6,4.1333252667878,4.73766653034721));
#26675=CARTESIAN_POINT('Origin',(3.95,3.01332647475228,5.61762046514307));
#26676=CARTESIAN_POINT('',(0.6,2.7249038366124,5.63627202561129));
#26677=CARTESIAN_POINT('',(0.6,2.79527803907584,5.63172110443148));
#26678=CARTESIAN_POINT('',(3.95,2.7249038366124,5.63627202561129));
#26679=CARTESIAN_POINT('Origin',(3.95,1.8415139408087,6.10300110926129));
#26680=CARTESIAN_POINT('',(0.6,2.05864818897191,5.91224415087166));
#26681=CARTESIAN_POINT('',(3.95,2.05864818897191,5.91224415087166));
#26682=CARTESIAN_POINT('',(0.6,2.00566812596253,5.95878823942725));
#26683=CARTESIAN_POINT('Origin',(3.95,0.634180373472706,6.34315468735702));
#26684=CARTESIAN_POINT('',(0.6,0.360574958203414,6.25001191718784));
#26685=CARTESIAN_POINT('',(0.6,0.427333805613703,6.2727384556044));
#26686=CARTESIAN_POINT('',(3.95,0.360574958203414,6.25001191718784));
#26687=CARTESIAN_POINT('Origin',(3.95,-0.634180373472705,6.34315468735702));
#26688=CARTESIAN_POINT('',(0.6,-0.360574958203413,6.25001191718784));
#26689=CARTESIAN_POINT('',(3.95,-0.360574958203413,6.25001191718784));
#26690=CARTESIAN_POINT('',(0.6,-0.427333805613702,6.2727384556044));
#26691=CARTESIAN_POINT('Origin',(3.95,-1.84151394080869,6.10300110926129));
#26692=CARTESIAN_POINT('',(0.6,-2.05864818897191,5.91224415087166));
#26693=CARTESIAN_POINT('',(0.6,-2.00566812596253,5.95878823942725));
#26694=CARTESIAN_POINT('',(3.95,-2.05864818897191,5.91224415087166));
#26695=CARTESIAN_POINT('Origin',(3.95,-3.01332647475229,5.61762046514307));
#26696=CARTESIAN_POINT('',(0.6,-2.7249038366124,5.63627202561129));
#26697=CARTESIAN_POINT('',(3.95,-2.7249038366124,5.63627202561129));
#26698=CARTESIAN_POINT('',(0.6,-2.79527803907584,5.63172110443148));
#26699=CARTESIAN_POINT('Origin',(3.95,-4.03685445096741,4.93372093612335));
#26700=CARTESIAN_POINT('',(0.6,-4.16446081106857,4.67439080721195));
#26701=CARTESIAN_POINT('',(0.6,-4.1333252667878,4.73766653034721));
#26702=CARTESIAN_POINT('',(3.95,-4.16446081106857,4.67439080721195));
#26703=CARTESIAN_POINT('Origin',(3.95,-4.93372093612335,4.03685445096741));
#26704=CARTESIAN_POINT('',(0.6,-4.67439080721195,4.16446081106857));
#26705=CARTESIAN_POINT('',(3.95,-4.67439080721195,4.16446081106857));
#26706=CARTESIAN_POINT('',(0.6,-4.73766653034721,4.1333252667878));
#26707=CARTESIAN_POINT('Origin',(3.95,-5.61762046514307,3.01332647475228));
#26708=CARTESIAN_POINT('',(0.6,-5.63627202561129,2.7249038366124));
#26709=CARTESIAN_POINT('',(0.6,-5.63172110443148,2.79527803907584));
#26710=CARTESIAN_POINT('',(3.95,-5.63627202561129,2.7249038366124));
#26711=CARTESIAN_POINT('Origin',(3.95,-6.10300110926129,1.8415139408087));
#26712=CARTESIAN_POINT('',(0.6,-5.91224415087166,2.05864818897191));
#26713=CARTESIAN_POINT('',(3.95,-5.91224415087166,2.05864818897191));
#26714=CARTESIAN_POINT('',(0.6,-5.95878823942725,2.00566812596253));
#26715=CARTESIAN_POINT('Origin',(3.95,-6.34315468735702,0.634180373472706));
#26716=CARTESIAN_POINT('',(0.6,-6.25001191718784,0.360574958203414));
#26717=CARTESIAN_POINT('',(0.6,-6.2727384556044,0.427333805613704));
#26718=CARTESIAN_POINT('',(3.95,-6.25001191718784,0.360574958203414));
#26719=CARTESIAN_POINT('Origin',(3.95,-6.34315468735702,-0.634180373472705));
#26720=CARTESIAN_POINT('',(0.6,-6.25001191718784,-0.360574958203412));
#26721=CARTESIAN_POINT('',(3.95,-6.25001191718784,-0.360574958203413));
#26722=CARTESIAN_POINT('',(0.6,-6.2727384556044,-0.427333805613702));
#26723=CARTESIAN_POINT('Origin',(3.95,-6.10300110926129,-1.84151394080869));
#26724=CARTESIAN_POINT('',(0.6,-5.91224415087166,-2.05864818897191));
#26725=CARTESIAN_POINT('',(0.6,-5.95878823942725,-2.00566812596253));
#26726=CARTESIAN_POINT('',(3.95,-5.91224415087166,-2.05864818897191));
#26727=CARTESIAN_POINT('Origin',(3.95,-5.61762046514307,-3.01332647475229));
#26728=CARTESIAN_POINT('',(0.6,-5.6362720256113,-2.7249038366124));
#26729=CARTESIAN_POINT('',(3.95,-5.6362720256113,-2.7249038366124));
#26730=CARTESIAN_POINT('',(0.6,-5.63172110443148,-2.79527803907584));
#26731=CARTESIAN_POINT('Origin',(3.95,-4.93372093612335,-4.03685445096742));
#26732=CARTESIAN_POINT('',(0.6,-4.67439080721195,-4.16446081106857));
#26733=CARTESIAN_POINT('',(0.6,-4.73766653034721,-4.1333252667878));
#26734=CARTESIAN_POINT('',(3.95,-4.67439080721195,-4.16446081106857));
#26735=CARTESIAN_POINT('Origin',(3.95,-4.03685445096742,-4.93372093612334));
#26736=CARTESIAN_POINT('',(0.6,-4.16446081106857,-4.67439080721194));
#26737=CARTESIAN_POINT('',(3.95,-4.16446081106857,-4.67439080721194));
#26738=CARTESIAN_POINT('',(0.6,-4.1333252667878,-4.73766653034721));
#26739=CARTESIAN_POINT('Origin',(3.95,-3.01332647475229,-5.61762046514307));
#26740=CARTESIAN_POINT('',(0.6,-2.72490383661241,-5.63627202561129));
#26741=CARTESIAN_POINT('',(0.6,-2.79527803907584,-5.63172110443147));
#26742=CARTESIAN_POINT('',(3.95,-2.72490383661241,-5.63627202561129));
#26743=CARTESIAN_POINT('Origin',(3.95,-1.8415139408087,-6.10300110926129));
#26744=CARTESIAN_POINT('',(0.6,-2.05864818897192,-5.91224415087166));
#26745=CARTESIAN_POINT('',(3.95,-2.05864818897192,-5.91224415087166));
#26746=CARTESIAN_POINT('',(0.6,-2.00566812596253,-5.95878823942725));
#26747=CARTESIAN_POINT('Origin',(3.95,-0.634180373472707,-6.34315468735702));
#26748=CARTESIAN_POINT('',(0.6,-0.360574958203415,-6.25001191718784));
#26749=CARTESIAN_POINT('',(0.6,-0.427333805613704,-6.2727384556044));
#26750=CARTESIAN_POINT('',(3.95,-0.360574958203415,-6.25001191718784));
#26751=CARTESIAN_POINT('Origin',(3.95,0.634180373472704,-6.34315468735702));
#26752=CARTESIAN_POINT('',(0.6,0.360574958203412,-6.25001191718784));
#26753=CARTESIAN_POINT('',(3.95,0.360574958203412,-6.25001191718784));
#26754=CARTESIAN_POINT('',(0.6,0.427333805613702,-6.2727384556044));
#26755=CARTESIAN_POINT('Origin',(3.95,1.8415139408087,-6.10300110926129));
#26756=CARTESIAN_POINT('',(0.6,2.05864818897191,-5.91224415087166));
#26757=CARTESIAN_POINT('',(0.6,2.00566812596253,-5.95878823942725));
#26758=CARTESIAN_POINT('',(3.95,2.05864818897191,-5.91224415087166));
#26759=CARTESIAN_POINT('Origin',(3.95,3.01332647475229,-5.61762046514307));
#26760=CARTESIAN_POINT('',(0.6,2.72490383661241,-5.63627202561129));
#26761=CARTESIAN_POINT('',(3.95,2.72490383661241,-5.63627202561129));
#26762=CARTESIAN_POINT('',(0.6,2.79527803907584,-5.63172110443148));
#26763=CARTESIAN_POINT('Origin',(3.95,4.03685445096741,-4.93372093612335));
#26764=CARTESIAN_POINT('',(0.6,4.16446081106857,-4.67439080721195));
#26765=CARTESIAN_POINT('',(0.6,4.1333252667878,-4.73766653034721));
#26766=CARTESIAN_POINT('',(3.95,4.16446081106857,-4.67439080721195));
#26767=CARTESIAN_POINT('Origin',(3.95,4.93372093612335,-4.03685445096741));
#26768=CARTESIAN_POINT('',(0.6,4.67439080721195,-4.16446081106857));
#26769=CARTESIAN_POINT('',(3.95,4.67439080721195,-4.16446081106857));
#26770=CARTESIAN_POINT('',(0.6,4.7376665303472,-4.1333252667878));
#26771=CARTESIAN_POINT('Ctrl Pts',(7.39428617940509,5.5955384738582,-3.31877409641756));
#26772=CARTESIAN_POINT('Ctrl Pts',(7.46976289566289,5.54381939543681,-3.25801858335938));
#26773=CARTESIAN_POINT('Ctrl Pts',(7.62033583663474,5.45380336720261,-3.11382584884576));
#26774=CARTESIAN_POINT('Ctrl Pts',(7.81463329279646,5.37650527564507,-2.85267802239966));
#26775=CARTESIAN_POINT('Ctrl Pts',(7.98425119443302,5.38246983194813,-2.46771855869631));
#26776=CARTESIAN_POINT('Ctrl Pts',(7.97308777074854,5.61920950447284,-1.91938073772091));
#26777=CARTESIAN_POINT('Ctrl Pts',(7.67997347882042,5.99409705965181,-1.66087268674238));
#26778=CARTESIAN_POINT('Ctrl Pts',(7.4697628956628,6.22383932171217,-1.61630525466166));
#26779=CARTESIAN_POINT('Ctrl Pts',(7.394286179405,6.30337086805857,-1.60991553045225));
#26780=CARTESIAN_POINT('Ctrl Pts',(7.29765887109684,5.62436223494091,-3.17572382553274));
#26781=CARTESIAN_POINT('Ctrl Pts',(7.36647595579574,5.5822650494995,-3.11685834537302));
#26782=CARTESIAN_POINT('Ctrl Pts',(7.501350054236,5.5120996672264,-2.98212215980868));
#26783=CARTESIAN_POINT('Ctrl Pts',(7.66846140186336,5.45952849244207,-2.75326447440463));
#26784=CARTESIAN_POINT('Ctrl Pts',(7.80024313771858,5.47482631338047,-2.44676755506769));
#26785=CARTESIAN_POINT('Ctrl Pts',(7.79287204927538,5.65171340584687,-2.03492319836375));
#26786=CARTESIAN_POINT('Ctrl Pts',(7.55870439802978,5.9466451212402,-1.80165889219619));
#26787=CARTESIAN_POINT('Ctrl Pts',(7.36647595579565,6.15120914289298,-1.7433057988706));
#26788=CARTESIAN_POINT('Ctrl Pts',(7.29765887109675,6.22260052838622,-1.73144882396635));
#26789=CARTESIAN_POINT('Ctrl Pts',(7.20103156278858,5.65318599602361,-3.03267355464793));
#26790=CARTESIAN_POINT('Ctrl Pts',(7.26318901592858,5.62071070356219,-2.97569810738666));
#26791=CARTESIAN_POINT('Ctrl Pts',(7.38236427183726,5.57039596725019,-2.8504184707716));
#26792=CARTESIAN_POINT('Ctrl Pts',(7.52228951093026,5.54255170923908,-2.6538509264096));
#26793=CARTESIAN_POINT('Ctrl Pts',(7.61623508100414,5.56718279481282,-2.42581655143907));
#26794=CARTESIAN_POINT('Ctrl Pts',(7.61265632780222,5.6842173072209,-2.15046565900658));
#26795=CARTESIAN_POINT('Ctrl Pts',(7.43743531723913,5.89919318282859,-1.94244509765));
#26796=CARTESIAN_POINT('Ctrl Pts',(7.26318901592851,6.07857896407379,-1.87030634307954));
#26797=CARTESIAN_POINT('Ctrl Pts',(7.2010315627885,6.14183018871386,-1.85298211748045));
#26798=CARTESIAN_POINT('Ctrl Pts',(7.10440425448033,5.68200975710631,-2.88962328376311));
#26799=CARTESIAN_POINT('Ctrl Pts',(7.15990207606142,5.65915635762488,-2.8345378694003));
#26800=CARTESIAN_POINT('Ctrl Pts',(7.26337848943852,5.62869226727397,-2.71871478173452));
#26801=CARTESIAN_POINT('Ctrl Pts',(7.37611761999717,5.62557492603609,-2.55443737841458));
#26802=CARTESIAN_POINT('Ctrl Pts',(7.43222702428969,5.65953927624516,-2.40486554781045));
#26803=CARTESIAN_POINT('Ctrl Pts',(7.43244060632906,5.71672120859493,-2.26600811964941));
#26804=CARTESIAN_POINT('Ctrl Pts',(7.31616623644848,5.85174124441698,-2.08323130310381));
#26805=CARTESIAN_POINT('Ctrl Pts',(7.15990207606136,6.0059487852546,-1.99730688728848));
#26806=CARTESIAN_POINT('Ctrl Pts',(7.10440425448025,6.06105984904151,-1.97451541099454));
#26807=CARTESIAN_POINT('',(7.25292710453826,5.63627202561129,-2.72490383661241));
#26808=CARTESIAN_POINT('',(7.25292710453827,5.91224415087166,-2.05864818897192));
#26809=CARTESIAN_POINT('Ctrl Pts',(7.25269877985884,5.63645713070299,-2.72481700882979));
#26810=CARTESIAN_POINT('Ctrl Pts',(7.25390396092312,5.6362292427284,-2.72330726216592));
#26811=CARTESIAN_POINT('Ctrl Pts',(7.29995254002791,5.62768096094605,-2.66542104042265));
#26812=CARTESIAN_POINT('Ctrl Pts',(7.37611761999717,5.62557492603609,-2.55443737841458));
#26813=CARTESIAN_POINT('Ctrl Pts',(7.43222702428969,5.65953927624516,-2.40486554781045));
#26814=CARTESIAN_POINT('Ctrl Pts',(7.43244060632906,5.71672120859493,-2.26600811964941));
#26815=CARTESIAN_POINT('Ctrl Pts',(7.3444569328455,5.81888954335097,-2.12770269805194));
#26816=CARTESIAN_POINT('Ctrl Pts',(7.25402238610438,5.91146676762003,-2.0584409850931));
#26817=CARTESIAN_POINT('Ctrl Pts',(7.25282290367468,5.91269329897841,-2.05753054923321));
#26818=CARTESIAN_POINT('Ctrl Pts',(7.25292710457906,5.91224415071533,-2.05864818914986));
#26819=CARTESIAN_POINT('Ctrl Pts',(7.2457805786392,5.93962960438486,-2.0274759585621));
#26820=CARTESIAN_POINT('Ctrl Pts',(7.24511949066774,5.96740428223051,-1.99586068306754));
#26821=CARTESIAN_POINT('Ctrl Pts',(7.25392829017846,6.03832444366435,-1.91513389824904));
#26822=CARTESIAN_POINT('Ctrl Pts',(7.2698369054514,6.08532226073065,-1.86163736653582));
#26823=CARTESIAN_POINT('Ctrl Pts',(7.31848027241684,6.18902485431357,-1.74359509494429));
#26824=CARTESIAN_POINT('Ctrl Pts',(7.35068643968617,6.24363465640856,-1.68143401615411));
#26825=CARTESIAN_POINT('Ctrl Pts',(7.38278617788903,6.2937580676509,-1.6243796926455));
#26826=CARTESIAN_POINT('Ctrl Pts',(7.38278617788903,5.59896890467484,-3.30174911289214));
#26827=CARTESIAN_POINT('Ctrl Pts',(7.36731678113116,5.6013307273702,-3.26522653164345));
#26828=CARTESIAN_POINT('Ctrl Pts',(7.35173106112422,5.60381146615418,-3.22690841479602));
#26829=CARTESIAN_POINT('Ctrl Pts',(7.33695451365628,5.60633295692038,-3.18798774492175));
#26830=CARTESIAN_POINT('Ctrl Pts',(7.32259692411982,5.60878295611807,-3.15017058879979));
#26831=CARTESIAN_POINT('Ctrl Pts',(7.30900069055514,5.61127616857016,-3.11178444084887));
#26832=CARTESIAN_POINT('Ctrl Pts',(7.2969989223891,5.61374501140461,-3.07394552961325));
#26833=CARTESIAN_POINT('Ctrl Pts',(7.29357288432376,5.61444977002109,-3.06314399200224));
#26834=CARTESIAN_POINT('Ctrl Pts',(7.29027681897695,5.61515230894107,-3.05238718446692));
#26835=CARTESIAN_POINT('Ctrl Pts',(7.28713040024107,5.61585016846552,-3.04170135195279));
#26836=CARTESIAN_POINT('Ctrl Pts',(7.27893276765674,5.61766836129272,-3.01386064282861));
#26837=CARTESIAN_POINT('Ctrl Pts',(7.27135734706788,5.61954609460126,-2.98524259075305));
#26838=CARTESIAN_POINT('Ctrl Pts',(7.26502754488307,5.62143232079745,-2.9564658321727));
#26839=CARTESIAN_POINT('Ctrl Pts',(7.26120721380904,5.62257074635002,-2.93909771515981));
#26840=CARTESIAN_POINT('Ctrl Pts',(7.25783974476678,5.62371308308983,-2.92167233545939));
#26841=CARTESIAN_POINT('Ctrl Pts',(7.25505700589891,5.62484873636172,-2.90433061300932));
#26842=CARTESIAN_POINT('Ctrl Pts',(7.25030000552081,5.62679009819994,-2.87468551004808));
#26843=CARTESIAN_POINT('Ctrl Pts',(7.24751313230281,5.62860295175123,-2.8470768605835));
#26844=CARTESIAN_POINT('Ctrl Pts',(7.24659919942187,5.63028834819705,-2.82113721885073));
#26845=CARTESIAN_POINT('Ctrl Pts',(7.2457555035245,5.6318442196362,-2.79719107382705));
#26846=CARTESIAN_POINT('Ctrl Pts',(7.24650820132933,5.63329170331371,-2.77466707014329));
#26847=CARTESIAN_POINT('Ctrl Pts',(7.24874445844377,5.63465189072976,-2.75328833157376));
#26848=CARTESIAN_POINT('Ctrl Pts',(7.24976108840657,5.63527024864274,-2.74356929432347));
#26849=CARTESIAN_POINT('Ctrl Pts',(7.25108378598209,5.63587083484386,-2.7340871419125));
#26850=CARTESIAN_POINT('Ctrl Pts',(7.25269878003204,5.63645713067024,-2.72481700861281));
#26851=CARTESIAN_POINT('Origin',(3.95,6.10300110926129,-1.8415139408087));
#26852=CARTESIAN_POINT('',(0.6,5.91224415087166,-2.05864818897192));
#26853=CARTESIAN_POINT('',(3.95,5.91224415087166,-2.05864818897192));
#26854=CARTESIAN_POINT('',(0.6,5.95878823942725,-2.00566812596253));
#26855=CARTESIAN_POINT('Origin',(3.95,5.61762046514307,-3.01332647475229));
#26856=CARTESIAN_POINT('',(0.6,5.63627202561129,-2.72490383661241));
#26857=CARTESIAN_POINT('',(0.6,5.63172110443147,-2.79527803907584));
#26858=CARTESIAN_POINT('',(3.95,5.63627202561129,-2.72490383661241));
#26859=CARTESIAN_POINT('Origin',(0.6,6.32857479770231,-2.62138151170087));
#26860=CARTESIAN_POINT('Origin',(0.6,6.32857479770231,-2.62138151170087));
#26861=CARTESIAN_POINT('Origin',(3.16,0.,0.));
#26862=CARTESIAN_POINT('',(3.,-2.47,3.02487759389396E-16));
#26863=CARTESIAN_POINT('',(3.16,-2.31,-2.82893410603039E-16));
#26864=CARTESIAN_POINT('Origin',(3.,0.,0.));
#26865=CARTESIAN_POINT('Origin',(3.,0.,0.));
#26866=CARTESIAN_POINT('',(3.,3.55,-2.04959345562317));
#26867=CARTESIAN_POINT('',(3.,3.55,2.04959345562317));
#26868=CARTESIAN_POINT('',(3.,3.55,-2.04959345562317));
#26869=CARTESIAN_POINT('',(3.,-5.55111512312578E-16,-4.09918691124634));
#26870=CARTESIAN_POINT('',(3.,-7.53008419494684E-16,-4.09918691124634));
#26871=CARTESIAN_POINT('',(3.,-3.55,-2.04959345562317));
#26872=CARTESIAN_POINT('',(3.,-3.55,-2.04959345562317));
#26873=CARTESIAN_POINT('',(3.,-3.55,2.04959345562317));
#26874=CARTESIAN_POINT('',(3.,-3.55,2.04959345562317));
#26875=CARTESIAN_POINT('',(3.,0.,4.09918691124634));
#26876=CARTESIAN_POINT('',(3.,2.51002806498228E-16,4.09918691124634));
#26877=CARTESIAN_POINT('',(3.,3.55,2.04959345562317));
#26878=CARTESIAN_POINT('Origin',(0.16,1.2825,5.02439071762272));
#26879=CARTESIAN_POINT('',(0.,-3.87,2.23434554176385));
#26880=CARTESIAN_POINT('',(0.,-1.11022302462516E-15,4.4686910835277));
#26881=CARTESIAN_POINT('',(0.,1.2025,5.16295478222823));
#26882=CARTESIAN_POINT('',(0.32,2.51002806498228E-16,4.09918691124634));
#26883=CARTESIAN_POINT('',(0.,-1.11022302462516E-15,4.4686910835277));
#26884=CARTESIAN_POINT('',(0.32,-3.55,2.04959345562317));
#26885=CARTESIAN_POINT('',(0.32,1.3625,4.88582665301721));
#26886=CARTESIAN_POINT('',(0.,-3.87,2.23434554176385));
#26887=CARTESIAN_POINT('Origin',(0.16,4.9925,1.40151777845782));
#26888=CARTESIAN_POINT('',(0.,3.87,2.23434554176385));
#26889=CARTESIAN_POINT('',(0.,5.0725,1.54008184306333));
#26890=CARTESIAN_POINT('',(0.32,3.55,2.04959345562317));
#26891=CARTESIAN_POINT('',(0.,3.87,2.23434554176385));
#26892=CARTESIAN_POINT('',(0.32,4.9125,1.26295371385231));
#26893=CARTESIAN_POINT('Origin',(0.16,3.2175,-2.4263145062694));
#26894=CARTESIAN_POINT('',(0.,3.87,-2.23434554176385));
#26895=CARTESIAN_POINT('',(0.,-2.98372437868011E-15,-4.4686910835277));
#26896=CARTESIAN_POINT('',(0.,3.2975,-2.56487857087491));
#26897=CARTESIAN_POINT('',(0.32,-7.53008419494684E-16,-4.09918691124634));
#26898=CARTESIAN_POINT('',(0.,-3.2612801348364E-15,-4.4686910835277));
#26899=CARTESIAN_POINT('',(0.32,3.55,-2.04959345562317));
#26900=CARTESIAN_POINT('',(0.32,3.1375,-2.28775044166389));
#26901=CARTESIAN_POINT('',(0.32,3.55,-2.04959345562317));
#26902=CARTESIAN_POINT('Origin',(0.16,-0.492500000000001,-3.99959398981113));
#26903=CARTESIAN_POINT('',(0.32,-3.55,-2.04959345562317));
#26904=CARTESIAN_POINT('',(0.32,-0.4125,-3.86102992520562));
#26905=CARTESIAN_POINT('',(0.,-3.87,-2.23434554176385));
#26906=CARTESIAN_POINT('',(0.,-0.572500000000001,-4.13815805441664));
#26907=CARTESIAN_POINT('',(0.,-3.87,-2.23434554176385));
#26908=CARTESIAN_POINT('Origin',(0.16,3.71,-1.02479672781159));
#26909=CARTESIAN_POINT('',(0.,3.87,-1.02479672781159));
#26910=CARTESIAN_POINT('',(0.32,3.55,-1.02479672781159));
#26911=CARTESIAN_POINT('Origin',(0.16,-3.71,1.02479672781158));
#26912=CARTESIAN_POINT('',(0.32,-3.55,1.02479672781158));
#26913=CARTESIAN_POINT('',(0.,-3.87,1.02479672781158));
#26914=CARTESIAN_POINT('Origin',(0.,3.55,2.04959345562317));
#26915=CARTESIAN_POINT('',(0.,3.55,2.04959345562317));
#26916=CARTESIAN_POINT('',(0.,2.51002806498228E-16,4.09918691124634));
#26917=CARTESIAN_POINT('Origin',(0.,3.55,-2.04959345562317));
#26918=CARTESIAN_POINT('',(0.,3.55,-2.04959345562317));
#26919=CARTESIAN_POINT('Origin',(0.,-7.53008419494684E-16,-4.09918691124634));
#26920=CARTESIAN_POINT('',(0.,-7.53008419494684E-16,-4.09918691124634));
#26921=CARTESIAN_POINT('Origin',(0.,6.,0.));
#26922=CARTESIAN_POINT('',(-6.93889390390723E-17,-6.,-7.34788079488412E-16));
#26923=CARTESIAN_POINT('Origin',(0.,0.,0.));
#26924=CARTESIAN_POINT('Origin',(0.,-3.55,-2.04959345562317));
#26925=CARTESIAN_POINT('',(0.,-3.55,-2.04959345562317));
#26926=CARTESIAN_POINT('Origin',(0.,-3.55,2.04959345562317));
#26927=CARTESIAN_POINT('',(0.,-3.55,2.04959345562317));
#26928=CARTESIAN_POINT('Origin',(0.,2.51002806498228E-16,4.09918691124634));
#26929=CARTESIAN_POINT('Origin',(0.6,6.32857479770231,-2.62138151170087));
#26930=CARTESIAN_POINT('Origin',(0.6,4.84368145112785,-4.84368145112785));
#26931=CARTESIAN_POINT('Origin',(0.6,4.84368145112785,-4.84368145112785));
#26932=CARTESIAN_POINT('Origin',(0.6,4.84368145112785,-4.84368145112785));
#26933=CARTESIAN_POINT('Origin',(0.6,2.62138151170087,-6.32857479770231));
#26934=CARTESIAN_POINT('Origin',(0.6,2.62138151170087,-6.32857479770231));
#26935=CARTESIAN_POINT('Origin',(0.6,2.62138151170087,-6.32857479770231));
#26936=CARTESIAN_POINT('Origin',(0.6,-1.25832458612391E-15,-6.85));
#26937=CARTESIAN_POINT('Origin',(0.6,-1.25832458612391E-15,-6.85));
#26938=CARTESIAN_POINT('Origin',(0.6,-1.25832458612391E-15,-6.85));
#26939=CARTESIAN_POINT('Origin',(0.6,-2.62138151170087,-6.32857479770231));
#26940=CARTESIAN_POINT('Origin',(0.6,-2.62138151170087,-6.32857479770231));
#26941=CARTESIAN_POINT('Origin',(0.6,-2.62138151170087,-6.32857479770231));
#26942=CARTESIAN_POINT('Origin',(0.6,-4.84368145112785,-4.84368145112785));
#26943=CARTESIAN_POINT('Origin',(0.6,-4.84368145112785,-4.84368145112785));
#26944=CARTESIAN_POINT('Origin',(0.6,-4.84368145112785,-4.84368145112785));
#26945=CARTESIAN_POINT('Origin',(0.6,-6.32857479770231,-2.62138151170086));
#26946=CARTESIAN_POINT('Origin',(0.6,-6.32857479770231,-2.62138151170086));
#26947=CARTESIAN_POINT('Origin',(0.6,-6.32857479770231,-2.62138151170086));
#26948=CARTESIAN_POINT('Origin',(0.6,-6.85,8.38883057415937E-16));
#26949=CARTESIAN_POINT('Origin',(0.6,-6.85,8.38883057415937E-16));
#26950=CARTESIAN_POINT('Origin',(0.6,-6.85,8.38883057415937E-16));
#26951=CARTESIAN_POINT('Origin',(0.6,-6.32857479770231,2.62138151170087));
#26952=CARTESIAN_POINT('Origin',(0.6,-6.32857479770231,2.62138151170087));
#26953=CARTESIAN_POINT('Origin',(0.6,-6.32857479770231,2.62138151170087));
#26954=CARTESIAN_POINT('Origin',(0.6,-4.84368145112785,4.84368145112785));
#26955=CARTESIAN_POINT('Origin',(0.6,-4.84368145112785,4.84368145112785));
#26956=CARTESIAN_POINT('Origin',(0.6,-4.84368145112785,4.84368145112785));
#26957=CARTESIAN_POINT('Origin',(0.6,-2.62138151170086,6.32857479770231));
#26958=CARTESIAN_POINT('Origin',(0.6,-2.62138151170086,6.32857479770231));
#26959=CARTESIAN_POINT('Origin',(0.6,-2.62138151170086,6.32857479770231));
#26960=CARTESIAN_POINT('Origin',(0.6,4.19441528707968E-16,6.85));
#26961=CARTESIAN_POINT('Origin',(0.6,4.19441528707968E-16,6.85));
#26962=CARTESIAN_POINT('Origin',(0.6,4.19441528707968E-16,6.85));
#26963=CARTESIAN_POINT('Origin',(0.6,2.62138151170087,6.32857479770231));
#26964=CARTESIAN_POINT('Origin',(0.6,2.62138151170087,6.32857479770231));
#26965=CARTESIAN_POINT('Origin',(0.6,2.62138151170087,6.32857479770231));
#26966=CARTESIAN_POINT('Origin',(0.6,4.84368145112785,4.84368145112785));
#26967=CARTESIAN_POINT('Origin',(0.6,4.84368145112785,4.84368145112785));
#26968=CARTESIAN_POINT('Origin',(0.6,4.84368145112785,4.84368145112785));
#26969=CARTESIAN_POINT('Origin',(0.6,6.32857479770231,2.62138151170086));
#26970=CARTESIAN_POINT('Origin',(0.6,6.32857479770231,2.62138151170086));
#26971=CARTESIAN_POINT('Origin',(0.6,6.32857479770231,2.62138151170086));
#26972=CARTESIAN_POINT('Origin',(0.6,6.85,0.));
#26973=CARTESIAN_POINT('Origin',(0.6,6.85,0.));
#26974=CARTESIAN_POINT('Origin',(0.6,6.85,0.));
#26975=CARTESIAN_POINT('Origin',(0.25,0.,0.));
#26976=CARTESIAN_POINT('',(0.25,-6.25,-7.65404249467096E-16));
#26977=CARTESIAN_POINT('',(0.,0.,0.));
#26978=CARTESIAN_POINT('Origin',(-7.7,0.,0.));
#26979=CARTESIAN_POINT('',(-15.4201303078758,-1.95627805222981,0.00129796472068854));
#26980=CARTESIAN_POINT('',(-15.5218696921242,-1.95584014130724,0.00207447844652431));
#26981=CARTESIAN_POINT('',(-7.7,-1.954,-2.39295984553393E-16));
#26982=CARTESIAN_POINT('',(-15.646,0.8625464214531,1.75510199459808));
#26983=CARTESIAN_POINT('Ctrl Pts',(-15.4201303078758,-1.95627805222981,
0.00129796472068854));
#26984=CARTESIAN_POINT('Ctrl Pts',(-15.4240829032361,-1.9567658369566,0.0703871063130427));
#26985=CARTESIAN_POINT('Ctrl Pts',(-15.4280354985964,-1.95342314936077,
0.139425514587532));
#26986=CARTESIAN_POINT('Ctrl Pts',(-15.4319880939568,-1.94609376501883,
0.20803425151521));
#26987=CARTESIAN_POINT('Ctrl Pts',(-15.4689952596497,-1.8774705653127,0.850400763642468));
#26988=CARTESIAN_POINT('Ctrl Pts',(-15.5060024253426,-1.45936912727697,
1.4551018111239));
#26989=CARTESIAN_POINT('Ctrl Pts',(-15.5430095910356,-0.882640818020853,
1.74666960837442));
#26990=CARTESIAN_POINT('Ctrl Pts',(-15.5773397273571,-0.347631959425933,
2.01714593475978));
#26991=CARTESIAN_POINT('Ctrl Pts',(-15.6116698636785,0.323884289759532,
2.01815339646098));
#26992=CARTESIAN_POINT('Ctrl Pts',(-15.646,0.863566983235696,1.7563826775686));
#26993=CARTESIAN_POINT('',(-15.646,-0.861525859670576,1.75382131162752));
#26994=CARTESIAN_POINT('Origin',(-15.646,0.,0.));
#26995=CARTESIAN_POINT('Ctrl Pts',(-15.646,-0.861525859670577,1.75382131162752));
#26996=CARTESIAN_POINT('Ctrl Pts',(-15.6089928343071,-1.44410240528909,
1.4676434918232));
#26997=CARTESIAN_POINT('Ctrl Pts',(-15.5719856686141,-1.86790219595322,
0.87091756707116));
#26998=CARTESIAN_POINT('Ctrl Pts',(-15.5349785029212,-1.94344388370824,
0.230308838951939));
#26999=CARTESIAN_POINT('Ctrl Pts',(-15.5306088993222,-1.95236343278762,
0.154669266141868));
#27000=CARTESIAN_POINT('Ctrl Pts',(-15.5262392957232,-1.95642770878322,
0.0784178971029367));
#27001=CARTESIAN_POINT('Ctrl Pts',(-15.5218696921242,-1.95584014130724,
0.00207447844652431));
#27002=CARTESIAN_POINT('Origin',(-7.7,0.,0.));
#27003=CARTESIAN_POINT('',(-14.7201303078758,-1.95121230271199,0.000898656016518479));
#27004=CARTESIAN_POINT('',(-14.8218696921242,-1.95111217225575,0.000805047651922751));
#27005=CARTESIAN_POINT('',(-7.7,-1.954,-2.39295984553393E-16));
#27006=CARTESIAN_POINT('Ctrl Pts',(-14.7201303078758,-1.95121230271199,
0.000898656016518479));
#27007=CARTESIAN_POINT('Ctrl Pts',(-14.7353732424118,-1.95232561653816,
0.269132749016255));
#27008=CARTESIAN_POINT('Ctrl Pts',(-14.7506161769478,-1.90081399086995,
0.536957184421699));
#27009=CARTESIAN_POINT('Ctrl Pts',(-14.7658591114838,-1.7946187287383,0.78098321012694));
#27010=CARTESIAN_POINT('Ctrl Pts',(-14.8028662771768,-1.53679529898949,
1.37343550632542));
#27011=CARTESIAN_POINT('Ctrl Pts',(-14.8398734428697,-0.956648445347352,
1.82561211140535));
#27012=CARTESIAN_POINT('Ctrl Pts',(-14.8768806085626,-0.319173913014248,
1.93098415809826));
#27013=CARTESIAN_POINT('Ctrl Pts',(-14.9138877742556,0.318300619318858,
2.03635620479117));
#27014=CARTESIAN_POINT('Ctrl Pts',(-14.9508949399485,1.01310283034293,1.79492369309705));
#27015=CARTESIAN_POINT('Ctrl Pts',(-14.9879021056415,1.447857066046,1.31693812925936));
#27016=CARTESIAN_POINT('Ctrl Pts',(-15.0249092713344,1.88261130174908,0.838952565421676));
#27017=CARTESIAN_POINT('Ctrl Pts',(-15.0619164370273,2.05731756213117,0.124413949440425));
#27018=CARTESIAN_POINT('Ctrl Pts',(-15.0989236027203,1.89218361321693,-0.500235697810672));
#27019=CARTESIAN_POINT('Ctrl Pts',(-15.1359307684132,1.72704966430269,-1.12488534506177));
#27020=CARTESIAN_POINT('Ctrl Pts',(-15.1729379341062,1.22207550609213,-1.65964602358271));
#27021=CARTESIAN_POINT('Ctrl Pts',(-15.2099450997991,0.607903721093593,
-1.86035794818561));
#27022=CARTESIAN_POINT('Ctrl Pts',(-15.2469522654921,-0.00626806390494887,
-2.06106987278851));
#27023=CARTESIAN_POINT('Ctrl Pts',(-15.283959431185,-0.729637475691471,
-1.92773304347336));
#27024=CARTESIAN_POINT('Ctrl Pts',(-15.3209665968779,-1.23174970089647,
-1.52104864042925));
#27025=CARTESIAN_POINT('Ctrl Pts',(-15.3540211672105,-1.68023321894303,
-1.1578006598858));
#27026=CARTESIAN_POINT('Ctrl Pts',(-15.3870757375432,-1.95219883007605,
-0.576477315011743));
#27027=CARTESIAN_POINT('Ctrl Pts',(-15.4201303078758,-1.95627805222981,
0.00129796472068854));
#27028=CARTESIAN_POINT('Ctrl Pts',(-15.5218696921242,-1.95584014130724,
0.00207447844652431));
#27029=CARTESIAN_POINT('Ctrl Pts',(-15.4892321300303,-1.95145146632858,
-0.568151861409059));
#27030=CARTESIAN_POINT('Ctrl Pts',(-15.4565945679363,-1.68753944404723,
-1.14351359006107));
#27031=CARTESIAN_POINT('Ctrl Pts',(-15.4239570058423,-1.24887387924439,
-1.50743054347954));
#27032=CARTESIAN_POINT('Ctrl Pts',(-15.3869498401494,-0.751478602179619,
-1.92006966630539));
#27033=CARTESIAN_POINT('Ctrl Pts',(-15.3499426744565,-0.0294044632041637,
-2.06085638047067));
#27034=CARTESIAN_POINT('Ctrl Pts',(-15.3129355087635,0.587041512969193,
-1.86689340445069));
#27035=CARTESIAN_POINT('Ctrl Pts',(-15.2759283430706,1.20348748914255,-1.67293042843072));
#27036=CARTESIAN_POINT('Ctrl Pts',(-15.2389211773776,1.71430530251381,-1.14421776222549));
#27037=CARTESIAN_POINT('Ctrl Pts',(-15.2019140116847,1.88641226529163,-0.521543698302765));
#27038=CARTESIAN_POINT('Ctrl Pts',(-15.1649068459917,2.05851922806946,0.10113036561996));
#27039=CARTESIAN_POINT('Ctrl Pts',(-15.1278996802988,1.89191534025386,0.817765827260178));
#27040=CARTESIAN_POINT('Ctrl Pts',(-15.0908925146059,1.46257189903353,1.30064584196409));
#27041=CARTESIAN_POINT('Ctrl Pts',(-15.0538853489129,1.03322845781319,1.78352585666799));
#27042=CARTESIAN_POINT('Ctrl Pts',(-15.01687818322,0.341145463188129,2.03265042443559));
#27043=CARTESIAN_POINT('Ctrl Pts',(-14.979871017527,-0.297480529695576,
1.93442073680281));
#27044=CARTESIAN_POINT('Ctrl Pts',(-14.9428638518341,-0.936106522579279,
1.83619104917002));
#27045=CARTESIAN_POINT('Ctrl Pts',(-14.9058566861412,-1.52127551372162,
1.39060710613685));
#27046=CARTESIAN_POINT('Ctrl Pts',(-14.8688495204482,-1.78573084508169,
0.801099057527319));
#27047=CARTESIAN_POINT('Ctrl Pts',(-14.8531895776736,-1.89763769549855,
0.551642982370853));
#27048=CARTESIAN_POINT('Ctrl Pts',(-14.8375296348989,-1.95211622085639,
0.276415256812969));
#27049=CARTESIAN_POINT('Ctrl Pts',(-14.8218696921242,-1.95111217225575,
0.000805047651922751));
#27050=CARTESIAN_POINT('Origin',(-7.7,0.,0.));
#27051=CARTESIAN_POINT('',(-14.0201303078758,-1.9530433091271,-0.00171791376288949));
#27052=CARTESIAN_POINT('',(-14.1218696921242,-1.95325151398278,-0.00174533096842624));
#27053=CARTESIAN_POINT('',(-7.7,-1.954,-2.39295984553393E-16));
#27054=CARTESIAN_POINT('Ctrl Pts',(-14.0201303078758,-1.9530433091271,-0.00171791376288949));
#27055=CARTESIAN_POINT('Ctrl Pts',(-14.0466635815875,-1.94908819668861,
0.464092547322558));
#27056=CARTESIAN_POINT('Ctrl Pts',(-14.0731968552992,-1.78205766518633,
0.932451059956011));
#27057=CARTESIAN_POINT('Ctrl Pts',(-14.0997301290109,-1.4785191386022,1.28240795655502));
#27058=CARTESIAN_POINT('Ctrl Pts',(-14.1367372947038,-1.05516012645965,
1.770508784163));
#27059=CARTESIAN_POINT('Ctrl Pts',(-14.1737444603967,-0.36625003980843,
2.02828115120971));
#27060=CARTESIAN_POINT('Ctrl Pts',(-14.2107516260897,0.273532057131348,
1.93798058286632));
#27061=CARTESIAN_POINT('Ctrl Pts',(-14.2477587917826,0.913314154071121,
1.84768001452293));
#27062=CARTESIAN_POINT('Ctrl Pts',(-14.2847659574756,1.50396826129945,1.40930651078944));
#27063=CARTESIAN_POINT('Ctrl Pts',(-14.3217731231685,1.77569634071135,0.823098916020689));
#27064=CARTESIAN_POINT('Ctrl Pts',(-14.3587802888615,2.04742442012326,0.236891321251938));
#27065=CARTESIAN_POINT('Ctrl Pts',(-14.3957874545544,2.00022647171874,-0.497150364552078));
#27066=CARTESIAN_POINT('Ctrl Pts',(-14.4327946202473,1.65566169603906,-1.04373070318105));
#27067=CARTESIAN_POINT('Ctrl Pts',(-14.4698017859403,1.31109692035938,-1.59031104181003));
#27068=CARTESIAN_POINT('Ctrl Pts',(-14.5068089516332,0.66916531740454,-1.94943003326396));
#27069=CARTESIAN_POINT('Ctrl Pts',(-14.5438161173262,0.0230868684858276,
-1.95705220165554));
#27070=CARTESIAN_POINT('Ctrl Pts',(-14.5808232830191,-0.622991580432885,
-1.96467437004712));
#27071=CARTESIAN_POINT('Ctrl Pts',(-14.617830448712,-1.27321687531547,-1.62079971537635));
#27072=CARTESIAN_POINT('Ctrl Pts',(-14.654837614405,-1.63057951982903,-1.08249839438246));
#27073=CARTESIAN_POINT('Ctrl Pts',(-14.6766018455619,-1.84074755232787,
-0.765918776278231));
#27074=CARTESIAN_POINT('Ctrl Pts',(-14.6983660767188,-1.94962268626342,
-0.38209247934674));
#27075=CARTESIAN_POINT('Ctrl Pts',(-14.7201303078758,-1.95121230271199,
0.000898656016518479));
#27076=CARTESIAN_POINT('Ctrl Pts',(-14.8218696921242,-1.95111217225575,
0.000805047651922751));
#27077=CARTESIAN_POINT('Ctrl Pts',(-14.800522469206,-1.94974347955955,-0.374899554732456));
#27078=CARTESIAN_POINT('Ctrl Pts',(-14.7791752462877,-1.8452747003299,-0.751314904469925));
#27079=CARTESIAN_POINT('Ctrl Pts',(-14.7578280233694,-1.64263463153156,
-1.06412750934765));
#27080=CARTESIAN_POINT('Ctrl Pts',(-14.7208208576765,-1.2913414150436,-1.60641387342718));
#27081=CARTESIAN_POINT('Ctrl Pts',(-14.6838136919835,-0.645013310489882,
-1.95755444740034));
#27082=CARTESIAN_POINT('Ctrl Pts',(-14.6468065262906,0.00111119976138999,
-1.95718427626721));
#27083=CARTESIAN_POINT('Ctrl Pts',(-14.6097993605976,0.647235710012662,
-1.95681410513408));
#27084=CARTESIAN_POINT('Ctrl Pts',(-14.5727921949047,1.29315662596149,-1.60493318889466));
#27085=CARTESIAN_POINT('Ctrl Pts',(-14.5357850292117,1.64383653694154,-1.06225813541516));
#27086=CARTESIAN_POINT('Ctrl Pts',(-14.4987778635188,1.9945164479216,-0.519583081935655));
#27087=CARTESIAN_POINT('Ctrl Pts',(-14.4617706978259,2.04995535393287,0.21388610878393));
#27088=CARTESIAN_POINT('Ctrl Pts',(-14.4247635321329,1.78482724106282,0.803108842016717));
#27089=CARTESIAN_POINT('Ctrl Pts',(-14.38775636644,1.51969912819276,1.39233157524951));
#27090=CARTESIAN_POINT('Ctrl Pts',(-14.350749200747,0.934003996441376,1.8373078509955));
#27091=CARTESIAN_POINT('Ctrl Pts',(-14.3137420350541,0.295276058031193,
1.93478632229321));
#27092=CARTESIAN_POINT('Ctrl Pts',(-14.2767348693612,-0.34345188037899,
2.03226479359092));
#27093=CARTESIAN_POINT('Ctrl Pts',(-14.2397277036682,-1.03521262544797,
1.78224546044036));
#27094=CARTESIAN_POINT('Ctrl Pts',(-14.2027205379753,-1.46402569115998,
1.29892954146499));
#27095=CARTESIAN_POINT('Ctrl Pts',(-14.1757702560249,-1.77630664563288,
0.946957158722955));
#27096=CARTESIAN_POINT('Ctrl Pts',(-14.1488199740746,-1.94913573752573,
0.471258095804866));
#27097=CARTESIAN_POINT('Ctrl Pts',(-14.1218696921242,-1.95325151398278,
-0.00174533096842624));
#27098=CARTESIAN_POINT('Origin',(-7.7,0.,0.));
#27099=CARTESIAN_POINT('',(-13.3201303078758,-1.95714464087111,0.00026399773373942));
#27100=CARTESIAN_POINT('',(-13.4218696921242,-1.95708965070517,0.000396557255078462));
#27101=CARTESIAN_POINT('',(-7.7,-1.954,-2.39295984553393E-16));
#27102=CARTESIAN_POINT('Ctrl Pts',(-13.3201303078758,-1.95714464087111,
0.00026399773373942));
#27103=CARTESIAN_POINT('Ctrl Pts',(-13.3209467550702,-1.95717172753317,
0.0145195559070077));
#27104=CARTESIAN_POINT('Ctrl Pts',(-13.3217632022646,-1.95702941419436,
0.0287745591326669));
#27105=CARTESIAN_POINT('Ctrl Pts',(-13.3225796494591,-1.95671604674699,
0.0430258010876729));
#27106=CARTESIAN_POINT('Ctrl Pts',(-13.359586815152,-1.94251201600704,0.688992957266154));
#27107=CARTESIAN_POINT('Ctrl Pts',(-13.396593980845,-1.57686979233981,1.32723241737986));
#27108=CARTESIAN_POINT('Ctrl Pts',(-13.4336011465379,-1.02680677935604,
1.66621029520631));
#27109=CARTESIAN_POINT('Ctrl Pts',(-13.4706083122308,-0.476743766372259,
2.00518817303275));
#27110=CARTESIAN_POINT('Ctrl Pts',(-13.5076154779238,0.257740035928053,
2.04490446857193));
#27111=CARTESIAN_POINT('Ctrl Pts',(-13.5446226436167,0.841148427119235,
1.76721765005178));
#27112=CARTESIAN_POINT('Ctrl Pts',(-13.5816298093097,1.42455681831042,1.48953083153163));
#27113=CARTESIAN_POINT('Ctrl Pts',(-13.6186369750026,1.85688979839247,0.894440898952159));
#27114=CARTESIAN_POINT('Ctrl Pts',(-13.6556441406956,1.94066707730226,0.253771957552514));
#27115=CARTESIAN_POINT('Ctrl Pts',(-13.6926513063885,2.02444435621205,-0.386896983847131));
#27116=CARTESIAN_POINT('Ctrl Pts',(-13.7296584720814,1.75966593394958,-1.07314493406695));
#27117=CARTESIAN_POINT('Ctrl Pts',(-13.7666656377744,1.26727683046446,-1.49150875303897));
#27118=CARTESIAN_POINT('Ctrl Pts',(-13.8036728034673,0.774887726979341,
-1.90987257201099));
#27119=CARTESIAN_POINT('Ctrl Pts',(-13.8406799691603,0.0548879422715688,
-2.06035225973521));
#27120=CARTESIAN_POINT('Ctrl Pts',(-13.8776871348532,-0.563842314011695,
-1.87421202025266));
#27121=CARTESIAN_POINT('Ctrl Pts',(-13.9146943005461,-1.18257257029496,
-1.68807178077012));
#27122=CARTESIAN_POINT('Ctrl Pts',(-13.9517014662391,-1.70003329815372,
-1.1653116140808));
#27123=CARTESIAN_POINT('Ctrl Pts',(-13.988708631932,-1.87985969326617,-0.544716886651509));
#27124=CARTESIAN_POINT('Ctrl Pts',(-13.9991825239133,-1.93075476189727,
-0.369074088357832));
#27125=CARTESIAN_POINT('Ctrl Pts',(-14.0096564158945,-1.9546045722002,-0.185594524925036));
#27126=CARTESIAN_POINT('Ctrl Pts',(-14.0201303078758,-1.9530433091271,-0.00171791376288949));
#27127=CARTESIAN_POINT('Ctrl Pts',(-14.1218696921242,-1.95325151398278,
-0.00174533096842624));
#27128=CARTESIAN_POINT('Ctrl Pts',(-14.1118128083816,-1.95478737492165,
-0.178253334917205));
#27129=CARTESIAN_POINT('Ctrl Pts',(-14.101755924639,-1.9328296346151,-0.354385967185775));
#27130=CARTESIAN_POINT('Ctrl Pts',(-14.0916990408964,-1.88585775871412,
-0.523573852172993));
#27131=CARTESIAN_POINT('Ctrl Pts',(-14.0546918752035,-1.7130113742012,-1.14614882203543));
#27132=CARTESIAN_POINT('Ctrl Pts',(-14.0176847095106,-1.20145321882029,
-1.67468625696012));
#27133=CARTESIAN_POINT('Ctrl Pts',(-13.9806775438176,-0.584852122809202,
-1.86776236812173));
#27134=CARTESIAN_POINT('Ctrl Pts',(-13.9436703781247,0.0317489732018875,
-2.06083847928334));
#27135=CARTESIAN_POINT('Ctrl Pts',(-13.9066632124317,0.753393009843159,
-1.91845326668187));
#27136=CARTESIAN_POINT('Ctrl Pts',(-13.8696560467388,1.25044882013409,-1.50564487944031));
#27137=CARTESIAN_POINT('Ctrl Pts',(-13.8326488810459,1.74750463042501,-1.09283649219875));
#27138=CARTESIAN_POINT('Ctrl Pts',(-13.7956417153529,2.0199722143656,-0.409604930317106));
#27139=CARTESIAN_POINT('Ctrl Pts',(-13.75863454966,1.94339425729846,0.231964346352179));
#27140=CARTESIAN_POINT('Ctrl Pts',(-13.721627383967,1.86681630023132,0.873533623021462));
#27141=CARTESIAN_POINT('Ctrl Pts',(-13.6846202182741,1.44119280215647,1.47344061447839));
#27142=CARTESIAN_POINT('Ctrl Pts',(-13.6476130525811,0.860939335837695,
1.75766096163323));
#27143=CARTESIAN_POINT('Ctrl Pts',(-13.6106058868882,0.280685869518923,
2.04188130878808));
#27144=CARTESIAN_POINT('Ctrl Pts',(-13.5735987211953,-0.454197565043769,
2.01041501164085));
#27145=CARTESIAN_POINT('Ctrl Pts',(-13.5365915555023,-1.00803223878929,
1.67763514366989));
#27146=CARTESIAN_POINT('Ctrl Pts',(-13.4995843898094,-1.56186691253481,
1.34485527569892));
#27147=CARTESIAN_POINT('Ctrl Pts',(-13.4625772241164,-1.93465282546315,
0.710761836904218));
#27148=CARTESIAN_POINT('Ctrl Pts',(-13.4255700584235,-1.95610948460737,
0.0649949216400037));
#27149=CARTESIAN_POINT('Ctrl Pts',(-13.4243366029904,-1.95682463888362,
0.0434713951763571));
#27150=CARTESIAN_POINT('Ctrl Pts',(-13.4231031475573,-1.9571495012145,0.0219349006384856));
#27151=CARTESIAN_POINT('Ctrl Pts',(-13.4218696921242,-1.95708965070517,
0.000396557255078462));
#27152=CARTESIAN_POINT('Origin',(-7.7,0.,0.));
#27153=CARTESIAN_POINT('',(-12.6201303078758,-1.95228596855585,0.00153407439264161));
#27154=CARTESIAN_POINT('',(-12.7218696921242,-1.95211097167562,0.00146895452558163));
#27155=CARTESIAN_POINT('',(-7.7,-1.954,-2.39295984553393E-16));
#27156=CARTESIAN_POINT('Ctrl Pts',(-12.6201303078758,-1.95228596855585,
0.00153407439264161));
#27157=CARTESIAN_POINT('Ctrl Pts',(-12.6322370942459,-1.95385293866565,
0.214285889020126));
#27158=CARTESIAN_POINT('Ctrl Pts',(-12.644343880616,-1.92179605864578,0.426578482544302));
#27159=CARTESIAN_POINT('Ctrl Pts',(-12.6564506669861,-1.85409897528216,
0.626822061414732));
#27160=CARTESIAN_POINT('Ctrl Pts',(-12.6934578326791,-1.64716733344281,
1.23891242756645));
#27161=CARTESIAN_POINT('Ctrl Pts',(-12.730464998372,-1.10722815379444,1.73842171037899));
#27162=CARTESIAN_POINT('Ctrl Pts',(-12.767472164065,-0.480913892112206,
1.89718495020391));
#27163=CARTESIAN_POINT('Ctrl Pts',(-12.8044793297579,0.145400369570025,
2.05594819002883));
#27164=CARTESIAN_POINT('Ctrl Pts',(-12.8414864954508,0.858089713286118,
1.87396538686614));
#27165=CARTESIAN_POINT('Ctrl Pts',(-12.8784936611438,1.331613171372,1.43436232121203));
#27166=CARTESIAN_POINT('Ctrl Pts',(-12.9155008268367,1.80513662945789,0.994759255557927));
#27167=CARTESIAN_POINT('Ctrl Pts',(-12.9525079925297,2.03949420191357,0.297535927412401));
#27168=CARTESIAN_POINT('Ctrl Pts',(-12.9895151582226,1.92763645460712,-0.338831234827492));
#27169=CARTESIAN_POINT('Ctrl Pts',(-13.0265223239155,1.81577870730067,-0.975198397067393));
#27170=CARTESIAN_POINT('Ctrl Pts',(-13.0635294896085,1.35770564023208,-1.55070939340166));
#27171=CARTESIAN_POINT('Ctrl Pts',(-13.1005366553014,0.762655052318492,
-1.80248333654236));
#27172=CARTESIAN_POINT('Ctrl Pts',(-13.1375438209944,0.167604464404906,
-2.05425727968306));
#27173=CARTESIAN_POINT('Ctrl Pts',(-13.1745509866873,-0.564423644353677,
-1.98229416963019));
#27174=CARTESIAN_POINT('Ctrl Pts',(-13.2115581523803,-1.09905477982664,
-1.61946518848213));
#27175=CARTESIAN_POINT('Ctrl Pts',(-13.2477488708788,-1.62189095390655,
-1.26464089232335));
#27176=CARTESIAN_POINT('Ctrl Pts',(-13.2839395893773,-1.95594396828844,
-0.631643241833467));
#27177=CARTESIAN_POINT('Ctrl Pts',(-13.3201303078758,-1.95714464087111,
0.00026399773373942));
#27178=CARTESIAN_POINT('Ctrl Pts',(-13.4218696921242,-1.95708965070517,
0.000396557255078462));
#27179=CARTESIAN_POINT('Ctrl Pts',(-13.3860959818644,-1.95535381597439,
-0.624276564294844));
#27180=CARTESIAN_POINT('Ctrl Pts',(-13.3503222716045,-1.63001111528494,
-1.25050486946977));
#27181=CARTESIAN_POINT('Ctrl Pts',(-13.3145485613447,-1.11717032068386,
-1.60702181624921));
#27182=CARTESIAN_POINT('Ctrl Pts',(-13.2775413956517,-0.58664709225607,
-1.97583124714049));
#27183=CARTESIAN_POINT('Ctrl Pts',(-13.2405342299588,0.1445267699596,-2.05600971718931));
#27184=CARTESIAN_POINT('Ctrl Pts',(-13.2035270642658,0.742366975175223,
-1.81093344118442));
#27185=CARTESIAN_POINT('Ctrl Pts',(-13.1665198985729,1.34020718039085,-1.56585716517953));
#27186=CARTESIAN_POINT('Ctrl Pts',(-13.12951273288,1.80471372860643,-0.995526143120937));
#27187=CARTESIAN_POINT('Ctrl Pts',(-13.092505567187,1.92371014573817,-0.36045516583733));
#27188=CARTESIAN_POINT('Ctrl Pts',(-13.0554984014941,2.04270656286991,0.274615811446275));
#27189=CARTESIAN_POINT('Ctrl Pts',(-13.0184912358011,1.8161928489178,0.974426743954891));
#27190=CARTESIAN_POINT('Ctrl Pts',(-12.9814840701082,1.34763553490042,1.41931924353683));
#27191=CARTESIAN_POINT('Ctrl Pts',(-12.9444769044152,0.87907822088303,1.86421174311878));
#27192=CARTESIAN_POINT('Ctrl Pts',(-12.9074697387223,0.168477306800354,
2.05418580977404));
#27193=CARTESIAN_POINT('Ctrl Pts',(-12.8704625730294,-0.459580189156903,
1.90246542710088));
#27194=CARTESIAN_POINT('Ctrl Pts',(-12.8334554073364,-1.08763768511415,
1.75074504442773));
#27195=CARTESIAN_POINT('Ctrl Pts',(-12.7964482416435,-1.63315176294599,
1.25733021242617));
#27196=CARTESIAN_POINT('Ctrl Pts',(-12.7594410759505,-1.84694347466266,
0.647602078798446));
#27197=CARTESIAN_POINT('Ctrl Pts',(-12.7469172813418,-1.91929388130583,
0.441260691400759));
#27198=CARTESIAN_POINT('Ctrl Pts',(-12.734393486733,-1.95365379066715,0.221598525482708));
#27199=CARTESIAN_POINT('Ctrl Pts',(-12.7218696921242,-1.95211097167562,
0.00146895452558163));
#27200=CARTESIAN_POINT('Origin',(-7.7,0.,0.));
#27201=CARTESIAN_POINT('',(-11.9201303078758,-1.95169843653047,-0.00126854855504954));
#27202=CARTESIAN_POINT('',(-12.0218696921242,-1.9518489925303,-0.00135048404527946));
#27203=CARTESIAN_POINT('',(-7.7,-1.954,-2.39295984553393E-16));
#27204=CARTESIAN_POINT('Ctrl Pts',(-11.9201303078758,-1.95169843653047,
-0.00126854855504954));
#27205=CARTESIAN_POINT('Ctrl Pts',(-11.9435274334216,-1.94924301286788,
0.410199212160575));
#27206=CARTESIAN_POINT('Ctrl Pts',(-11.9669245589674,-1.82209832848306,
0.823054588837745));
#27207=CARTESIAN_POINT('Ctrl Pts',(-11.9903216845132,-1.58142069241171,
1.15312510181565));
#27208=CARTESIAN_POINT('Ctrl Pts',(-12.0273288502061,-1.20074157269491,
1.67519667595913));
#27209=CARTESIAN_POINT('Ctrl Pts',(-12.0643360158991,-0.53602960573929,
1.99015991551352));
#27210=CARTESIAN_POINT('Ctrl Pts',(-12.101343181592,0.109089261378069,1.95414647349669));
#27211=CARTESIAN_POINT('Ctrl Pts',(-12.1383503472849,0.75420812849542,1.91813303147986));
#27212=CARTESIAN_POINT('Ctrl Pts',(-12.1753575129779,1.3797338957745,1.53114290789182));
#27213=CARTESIAN_POINT('Ctrl Pts',(-12.2123646786708,1.69994001855784,0.969944761380266));
#27214=CARTESIAN_POINT('Ctrl Pts',(-12.2493718443638,2.02014614134118,0.408746614868707));
#27215=CARTESIAN_POINT('Ctrl Pts',(-12.2863790100567,2.03503261962877,-0.326659554566366));
#27216=CARTESIAN_POINT('Ctrl Pts',(-12.3233861757497,1.73779963441016,-0.900356228093971));
#27217=CARTESIAN_POINT('Ctrl Pts',(-12.3603933414426,1.44056664919155,-1.47405290162158));
#27218=CARTESIAN_POINT('Ctrl Pts',(-12.3974005071355,0.831214200466734,
-1.88604007924171));
#27219=CARTESIAN_POINT('Ctrl Pts',(-12.4344076728285,0.18808121328365,-1.94813099252794));
#27220=CARTESIAN_POINT('Ctrl Pts',(-12.4714148385214,-0.455051773899431,
-2.01022190581416));
#27221=CARTESIAN_POINT('Ctrl Pts',(-12.5084220042144,-1.13196529954078,
-1.72241655476647));
#27222=CARTESIAN_POINT('Ctrl Pts',(-12.5454291699073,-1.5334600103463,-1.21617815449718));
#27223=CARTESIAN_POINT('Ctrl Pts',(-12.5703295492301,-1.80360689698215,
-0.875554171048228));
#27224=CARTESIAN_POINT('Ctrl Pts',(-12.5952299285529,-1.94906313559845,
-0.43603876483078));
#27225=CARTESIAN_POINT('Ctrl Pts',(-12.6201303078758,-1.95228596855585,
0.00153407439264161));
#27226=CARTESIAN_POINT('Ctrl Pts',(-12.7218696921242,-1.95211097167562,
0.00146895452558163));
#27227=CARTESIAN_POINT('Ctrl Pts',(-12.6973863210401,-1.94909484029808,
-0.428872977828815));
#27228=CARTESIAN_POINT('Ctrl Pts',(-12.6729029499559,-1.80886483995233,
-0.86100124945961));
#27229=CARTESIAN_POINT('Ctrl Pts',(-12.6484195788717,-1.54701966560394,
-1.19888231497363));
#27230=CARTESIAN_POINT('Ctrl Pts',(-12.6114124131788,-1.15123479922702,
-1.7095971398641));
#27231=CARTESIAN_POINT('Ctrl Pts',(-12.5744052474858,-0.477595720871672,
-2.00498535439116));
#27232=CARTESIAN_POINT('Ctrl Pts',(-12.5373980817929,0.166193912405789,
-1.95012005646431));
#27233=CARTESIAN_POINT('Ctrl Pts',(-12.5003909160999,0.809983545683245,
-1.89525475853747));
#27234=CARTESIAN_POINT('Ctrl Pts',(-12.463383750407,1.42392373388281,-1.49013594815671));
#27235=CARTESIAN_POINT('Ctrl Pts',(-12.4263765847141,1.7275799724757,-0.919813073269506));
#27236=CARTESIAN_POINT('Ctrl Pts',(-12.3893694190211,2.0312362110686,-0.349490198382288));
#27237=CARTESIAN_POINT('Ctrl Pts',(-12.3523622533282,2.02460850005481,0.386036741011393));
#27238=CARTESIAN_POINT('Ctrl Pts',(-12.3153550876352,1.71072423346732,0.950795061026896));
#27239=CARTESIAN_POINT('Ctrl Pts',(-12.2783479219423,1.39683996687984,1.51555338104239));
#27240=CARTESIAN_POINT('Ctrl Pts',(-12.2413407562494,0.775699144718677,
1.90954308167971));
#27241=CARTESIAN_POINT('Ctrl Pts',(-12.2043335905564,0.131025364222244,
1.95279824994973));
#27242=CARTESIAN_POINT('Ctrl Pts',(-12.1673264248635,-0.513648416274196,
1.99605341821975));
#27243=CARTESIAN_POINT('Ctrl Pts',(-12.1303192591705,-1.1818551551059,1.68857405412246));
#27244=CARTESIAN_POINT('Ctrl Pts',(-12.0933120934776,-1.56837256952603,
1.17081003336157));
#27245=CARTESIAN_POINT('Ctrl Pts',(-12.0694979596931,-1.81709676238617,
0.837628568953355));
#27246=CARTESIAN_POINT('Ctrl Pts',(-12.0456838259087,-1.94917536710479,
0.417369692204787));
#27247=CARTESIAN_POINT('Ctrl Pts',(-12.0218696921242,-1.9518489925303,-0.00135048404527946));
#27248=CARTESIAN_POINT('Origin',(-7.7,0.,0.));
#27249=CARTESIAN_POINT('',(-11.2201303078758,-1.95685610654859,-0.000727346471807722));
#27250=CARTESIAN_POINT('',(-11.3218696921242,-1.9569602541593,-0.00060337692984129));
#27251=CARTESIAN_POINT('',(-7.7,-1.954,-2.39295984553393E-16));
#27252=CARTESIAN_POINT('Ctrl Pts',(-11.2201303078758,-1.95685610654859,
-0.000727346471807722));
#27253=CARTESIAN_POINT('Ctrl Pts',(-11.2548177725973,-1.95395813312852,
0.60517099785977));
#27254=CARTESIAN_POINT('Ctrl Pts',(-11.2895052373187,-1.65063759095734,
1.21357459286489));
#27255=CARTESIAN_POINT('Ctrl Pts',(-11.3241927020402,-1.16369172863257,
1.57366148441711));
#27256=CARTESIAN_POINT('Ctrl Pts',(-11.3611998677332,-0.644181687894853,
1.95782894567513));
#27257=CARTESIAN_POINT('Ctrl Pts',(-11.3982070334261,0.0843345183607735,
2.0593571609984));
#27258=CARTESIAN_POINT('Ctrl Pts',(-11.435214199119,0.689086556393739,1.83187025321751));
#27259=CARTESIAN_POINT('Ctrl Pts',(-11.472221364812,1.29383859442671,1.60438334543661));
#27260=CARTESIAN_POINT('Ctrl Pts',(-11.5092285305049,1.77482646423702,1.04788131455156));
#27261=CARTESIAN_POINT('Ctrl Pts',(-11.5462356961979,1.91234538425969,0.416562165980472));
#27262=CARTESIAN_POINT('Ctrl Pts',(-11.5832428618908,2.04986430428237,-0.214756982590612));
#27263=CARTESIAN_POINT('Ctrl Pts',(-11.6202500275838,1.84391427451741,-0.92089324884772));
#27264=CARTESIAN_POINT('Ctrl Pts',(-11.6572571932767,1.38856878234954,-1.37929896813924));
#27265=CARTESIAN_POINT('Ctrl Pts',(-11.6942643589696,0.933223290181664,
-1.83770468743075));
#27266=CARTESIAN_POINT('Ctrl Pts',(-11.7312715246626,0.228482335610874,
-2.04837985975668));
#27267=CARTESIAN_POINT('Ctrl Pts',(-11.7682786903555,-0.403743764695274,
-1.91509265553802));
#27268=CARTESIAN_POINT('Ctrl Pts',(-11.8052858560485,-1.03596986500142,
-1.78180545131937));
#27269=CARTESIAN_POINT('Ctrl Pts',(-11.8422930217414,-1.59568111104292,
-1.30455587055615));
#27270=CARTESIAN_POINT('Ctrl Pts',(-11.8793001874343,-1.82721359782469,
-0.701341125808267));
#27271=CARTESIAN_POINT('Ctrl Pts',(-11.8929102275815,-1.91236376756786,
-0.479498227557532));
#27272=CARTESIAN_POINT('Ctrl Pts',(-11.9065202677286,-1.9531267493615,-0.240618152917035));
#27273=CARTESIAN_POINT('Ctrl Pts',(-11.9201303078758,-1.95169843653047,
-0.00126854855504954));
#27274=CARTESIAN_POINT('Ctrl Pts',(-12.0218696921242,-1.9518489925303,-0.00135048404527946));
#27275=CARTESIAN_POINT('Ctrl Pts',(-12.0086766602157,-1.95333018121721,
-0.233321493194773));
#27276=CARTESIAN_POINT('Ctrl Pts',(-11.9954836283072,-1.9150949004906,-0.464820250413784));
#27277=CARTESIAN_POINT('Ctrl Pts',(-11.9822905963988,-1.8349736515092,-0.680779222162789));
#27278=CARTESIAN_POINT('Ctrl Pts',(-11.9452834307058,-1.6102292290637,-1.28655577950177));
#27279=CARTESIAN_POINT('Ctrl Pts',(-11.9082762650129,-1.05591229416418,
-1.77006021675525));
#27280=CARTESIAN_POINT('Ctrl Pts',(-11.8712690993199,-0.425222747979457,
-1.91043823916569));
#27281=CARTESIAN_POINT('Ctrl Pts',(-11.834261933627,0.205466798205275,-2.05081626157613));
#27282=CARTESIAN_POINT('Ctrl Pts',(-11.797254767934,0.912528955675209,-1.84806786914353));
#27283=CARTESIAN_POINT('Ctrl Pts',(-11.7602476022411,1.37299313284074,-1.39480411106204));
#27284=CARTESIAN_POINT('Ctrl Pts',(-11.7232404365482,1.83345731000627,-0.941540352980555));
#27285=CARTESIAN_POINT('Ctrl Pts',(-11.6862332708552,2.04732350686741,-0.237761229250197));
#27286=CARTESIAN_POINT('Ctrl Pts',(-11.6492261051623,1.91690230334813,0.395062286838669));
#27287=CARTESIAN_POINT('Ctrl Pts',(-11.6122189394693,1.78648109982885,1.02788580292753));
#27288=CARTESIAN_POINT('Ctrl Pts',(-11.5752117737764,1.31177249592916,1.5897537113749));
#27289=CARTESIAN_POINT('Ctrl Pts',(-11.5382046080835,0.709613041327233,
1.82401699077679));
#27290=CARTESIAN_POINT('Ctrl Pts',(-11.5011974423905,0.107453586725291,
2.05828027017869));
#27291=CARTESIAN_POINT('Ctrl Pts',(-11.4641902766976,-0.622156718578892,
1.96493892053509));
#27292=CARTESIAN_POINT('Ctrl Pts',(-11.4271831110046,-1.14594778023205,
1.58662923710771));
#27293=CARTESIAN_POINT('Ctrl Pts',(-11.3920786380445,-1.64280855884786,
1.2277700323088));
#27294=CARTESIAN_POINT('Ctrl Pts',(-11.3569741650844,-1.95447007917529,
0.612492024699057));
#27295=CARTESIAN_POINT('Ctrl Pts',(-11.3218696921242,-1.9569602541593,-0.00060337692984129));
#27296=CARTESIAN_POINT('Origin',(-7.7,0.,0.));
#27297=CARTESIAN_POINT('',(-10.5201303078758,-1.95381282533802,0.00177708690787488));
#27298=CARTESIAN_POINT('',(-10.6218696921242,-1.95359472300144,0.00177181249679811));
#27299=CARTESIAN_POINT('',(-7.7,-1.954,-2.39295984553393E-16));
#27300=CARTESIAN_POINT('Ctrl Pts',(-10.5201303078758,-1.95381282533802,
0.00177708690787488));
#27301=CARTESIAN_POINT('Ctrl Pts',(-10.52910094608,-1.95524187263722,0.159105178249771));
#27302=CARTESIAN_POINT('Ctrl Pts',(-10.5380715842842,-1.93783046980655,
0.316120934930408));
#27303=CARTESIAN_POINT('Ctrl Pts',(-10.5470422224884,-1.90036359504,0.468195593179135));
#27304=CARTESIAN_POINT('Ctrl Pts',(-10.5840493881814,-1.74579902439106,
1.09555921518542));
#27305=CARTESIAN_POINT('Ctrl Pts',(-10.6210565538743,-1.24991750672224,
1.63883203957322));
#27306=CARTESIAN_POINT('Ctrl Pts',(-10.6580637195673,-0.639226917511803,
1.84985887428044));
#27307=CARTESIAN_POINT('Ctrl Pts',(-10.6950708852602,-0.0285363283013634,
2.06088570898765));
#27308=CARTESIAN_POINT('Ctrl Pts',(-10.7320780509531,0.696963332450705,
1.93966655401429));
#27309=CARTESIAN_POINT('Ctrl Pts',(-10.7690852166461,1.20587962328041,1.54157167883392));
#27310=CARTESIAN_POINT('Ctrl Pts',(-10.806092382339,1.71479591411012,1.14347680365354));
#27311=CARTESIAN_POINT('Ctrl Pts',(-10.843099548032,2.00712883501746,0.468506208266162));
#27312=CARTESIAN_POINT('Ctrl Pts',(-10.8801067137249,1.94934707562338,-0.175028242247616));
#27313=CARTESIAN_POINT('Ctrl Pts',(-10.9171138794179,1.89156531622931,-0.81856269276138));
#27314=CARTESIAN_POINT('Ctrl Pts',(-10.9541210451108,1.48366887653383,-1.43066099840154));
#27315=CARTESIAN_POINT('Ctrl Pts',(-10.9911282108037,0.911975964976942,
-1.73172998649619));
#27316=CARTESIAN_POINT('Ctrl Pts',(-11.0281353764967,0.340283053420042,
-2.03279897459085));
#27317=CARTESIAN_POINT('Ctrl Pts',(-11.0651425421896,-0.395206329998278,
-2.02283864513999));
#27318=CARTESIAN_POINT('Ctrl Pts',(-11.1021497078826,-0.958536656106322,
-1.70639865967078));
#27319=CARTESIAN_POINT('Ctrl Pts',(-11.1391568735755,-1.52186698221436,
-1.38995867420158));
#27320=CARTESIAN_POINT('Ctrl Pts',(-11.1761640392684,-1.91303825101214,
-0.767039032714035));
#27321=CARTESIAN_POINT('Ctrl Pts',(-11.2131712049614,-1.95337194780112,
-0.122175858373872));
#27322=CARTESIAN_POINT('Ctrl Pts',(-11.2154909059329,-1.95590016399579,
-0.0817542345081737));
#27323=CARTESIAN_POINT('Ctrl Pts',(-11.2178106069043,-1.95704990658016,
-0.0412463924510177));
#27324=CARTESIAN_POINT('Ctrl Pts',(-11.2201303078758,-1.95685610654859,
-0.000727346471807722));
#27325=CARTESIAN_POINT('Ctrl Pts',(-11.3218696921242,-1.9569602541593,-0.00060337692984129));
#27326=CARTESIAN_POINT('Ctrl Pts',(-11.3199669993914,-1.95709522379268,
-0.0338336768556207));
#27327=CARTESIAN_POINT('Ctrl Pts',(-11.3180643066586,-1.9563219303891,-0.0670575648665623));
#27328=CARTESIAN_POINT('Ctrl Pts',(-11.3161616139258,-1.95462063415894,
-0.100233864456555));
#27329=CARTESIAN_POINT('Ctrl Pts',(-11.2791544482329,-1.92153060843055,
-0.745509265382321));
#27330=CARTESIAN_POINT('Ctrl Pts',(-11.2421472825399,-1.53737873897162,
-1.3727820500227));
#27331=CARTESIAN_POINT('Ctrl Pts',(-11.205140116847,-0.977637231766315,
-1.69552767424427));
#27332=CARTESIAN_POINT('Ctrl Pts',(-11.168132951154,-0.41789572456102,-2.01827329846583));
#27333=CARTESIAN_POINT('Ctrl Pts',(-11.1311257854611,0.31743542039065,-2.0364917622686));
#27334=CARTESIAN_POINT('Ctrl Pts',(-11.0941186197681,0.892472953801631,
-1.7418612682405));
#27335=CARTESIAN_POINT('Ctrl Pts',(-11.0571114540752,1.46751048721262,-1.44723077421241));
#27336=CARTESIAN_POINT('Ctrl Pts',(-11.0201042883823,1.88225440908292,-0.839751322353458));
#27337=CARTESIAN_POINT('Ctrl Pts',(-10.9830971226893,1.94725873027388,-0.196906293540815));
#27338=CARTESIAN_POINT('Ctrl Pts',(-10.9460899569964,2.01226305146485,0.445938735271831));
#27339=CARTESIAN_POINT('Ctrl Pts',(-10.9090827913034,1.72752777197646,1.12414934103816));
#27340=CARTESIAN_POINT('Ctrl Pts',(-10.8720756256105,1.2231137650871,1.52793369251362));
#27341=CARTESIAN_POINT('Ctrl Pts',(-10.8350684599176,0.718699758197757,
1.93171804398907));
#27342=CARTESIAN_POINT('Ctrl Pts',(-10.7980612942246,-0.0053929760925614,
2.06107614117366));
#27343=CARTESIAN_POINT('Ctrl Pts',(-10.7610541285317,-0.618414649680478,
1.85692002308242));
#27344=CARTESIAN_POINT('Ctrl Pts',(-10.7240469628387,-1.23143632326841,
1.65276390499117));
#27345=CARTESIAN_POINT('Ctrl Pts',(-10.6870397971458,-1.73338693615394,
1.11509357162407));
#27346=CARTESIAN_POINT('Ctrl Pts',(-10.6500326314528,-1.89498638236701,
0.48950511918408));
#27347=CARTESIAN_POINT('Ctrl Pts',(-10.64064498501,-1.9359794829735,0.330811441884507));
#27348=CARTESIAN_POINT('Ctrl Pts',(-10.6312573385671,-1.95507132644295,
0.166460321563234));
#27349=CARTESIAN_POINT('Ctrl Pts',(-10.6218696921242,-1.95359472300144,
0.00177181249679811));
#27350=CARTESIAN_POINT('Origin',(-7.7,0.,0.));
#27351=CARTESIAN_POINT('',(-9.82013030787577,-1.95092775659677,-0.000499046442109796));
#27352=CARTESIAN_POINT('',(-9.92186969212424,-1.950990226885,-0.00061315819592252));
#27353=CARTESIAN_POINT('',(-7.7,-1.954,-2.39295984553393E-16));
#27354=CARTESIAN_POINT('Ctrl Pts',(-9.82013030787577,-1.95092775659677,
-0.000499046442109796));
#27355=CARTESIAN_POINT('Ctrl Pts',(-9.84039128525567,-1.95011071406785,
0.356168159601569));
#27356=CARTESIAN_POINT('Ctrl Pts',(-9.86065226263557,-1.85661555206154,
0.713234132722242));
#27357=CARTESIAN_POINT('Ctrl Pts',(-9.88091324001548,-1.67305055867318,
1.01562332335817));
#27358=CARTESIAN_POINT('Ctrl Pts',(-9.91792040570842,-1.33776465422886,
1.56794450075198));
#27359=CARTESIAN_POINT('Ctrl Pts',(-9.95492757140137,-0.701988617061191,
1.93785350557233));
#27360=CARTESIAN_POINT('Ctrl Pts',(-9.99193473709431,-0.0561310918315319,
1.95638396214944));
#27361=CARTESIAN_POINT('Ctrl Pts',(-10.0289419027873,0.589726433398127,
1.97491441872654));
#27362=CARTESIAN_POINT('Ctrl Pts',(-10.0659490684802,1.24566544668979,1.64206632706039));
#27363=CARTESIAN_POINT('Ctrl Pts',(-10.1029562341731,1.61206729509896,1.10987744499024));
#27364=CARTESIAN_POINT('Ctrl Pts',(-10.1399633998661,1.97846914350813,0.577688562920078));
#27365=CARTESIAN_POINT('Ctrl Pts',(-10.176970565559,2.05533382703483,-0.15384110955408));
#27366=CARTESIAN_POINT('Ctrl Pts',(-10.213977731252,1.80755123258835,-0.750564752965431));
#27367=CARTESIAN_POINT('Ctrl Pts',(-10.2509848969449,1.55976863814187,-1.34728839637677));
#27368=CARTESIAN_POINT('Ctrl Pts',(-10.2879920626378,0.987338765722227,
-1.8092060107253));
#27369=CARTESIAN_POINT('Ctrl Pts',(-10.3249992283308,0.351735111804125,
-1.92532369173338));
#27370=CARTESIAN_POINT('Ctrl Pts',(-10.3620063940237,-0.283868542113976,
-2.04144137274146));
#27371=CARTESIAN_POINT('Ctrl Pts',(-10.3990135597167,-0.982645977530532,
-1.81175912040909));
#27372=CARTESIAN_POINT('Ctrl Pts',(-10.4360207254096,-1.42541088342427,
-1.34119078443052));
#27373=CARTESIAN_POINT('Ctrl Pts',(-10.4640572528983,-1.76084836486043,
-0.984689500423752));
#27374=CARTESIAN_POINT('Ctrl Pts',(-10.492093780387,-1.94934652952108,-0.489930777932722));
#27375=CARTESIAN_POINT('Ctrl Pts',(-10.5201303078758,-1.95381282533802,
0.00177708690787488));
#27376=CARTESIAN_POINT('Ctrl Pts',(-10.6218696921242,-1.95359472300144,
0.00177181249679811));
#27377=CARTESIAN_POINT('Ctrl Pts',(-10.5942501728742,-1.94925038840961,
-0.48276043678513));
#27378=CARTESIAN_POINT('Ctrl Pts',(-10.5666306536241,-1.76686494916673,
-0.970213133349514));
#27379=CARTESIAN_POINT('Ctrl Pts',(-10.539011134374,-1.4403811131439,-1.3251003358094));
#27380=CARTESIAN_POINT('Ctrl Pts',(-10.5020039686811,-1.0029281181671,-1.80061076685003));
#27381=CARTESIAN_POINT('Ctrl Pts',(-10.4649968029881,-0.306773848672879,
-2.03812505741843));
#27382=CARTESIAN_POINT('Ctrl Pts',(-10.4279896372952,0.330093589370354,
-1.92915185335951));
#27383=CARTESIAN_POINT('Ctrl Pts',(-10.3909824716023,0.966961027413597,
-1.82017864930059));
#27384=CARTESIAN_POINT('Ctrl Pts',(-10.3539753059093,1.54454163400586,-1.36471795061433));
#27385=CARTESIAN_POINT('Ctrl Pts',(-10.3169681402164,1.79900916950086,-0.770814283154929));
#27386=CARTESIAN_POINT('Ctrl Pts',(-10.2799609745234,2.05347670499587,-0.176910615695531));
#27387=CARTESIAN_POINT('Ctrl Pts',(-10.2429538088305,1.98483116939363,0.555436020537005));
#27388=CARTESIAN_POINT('Ctrl Pts',(-10.2059466431375,1.62442834805074,1.09170563482698));
#27389=CARTESIAN_POINT('Ctrl Pts',(-10.1689394774446,1.26402552670786,1.62797524911695));
#27390=CARTESIAN_POINT('Ctrl Pts',(-10.1319323117517,0.611865419624326,
1.96816784146434));
#27391=CARTESIAN_POINT('Ctrl Pts',(-10.0949251460587,-0.0341594422952981,
1.95689084610407));
#27392=CARTESIAN_POINT('Ctrl Pts',(-10.0579179803658,-0.680184304214917,
1.9456138507438));
#27393=CARTESIAN_POINT('Ctrl Pts',(-10.0209108146728,-1.32007392097063,
1.58286726767587));
#27394=CARTESIAN_POINT('Ctrl Pts',(-9.98390364897989,-1.66154065435141,
1.03434583433266));
#27395=CARTESIAN_POINT('Ctrl Pts',(-9.96322566336134,-1.85233733034239,
0.727856047888396));
#27396=CARTESIAN_POINT('Ctrl Pts',(-9.94254767774279,-1.9499638271078,0.363365762621769));
#27397=CARTESIAN_POINT('Ctrl Pts',(-9.92186969212424,-1.950990226885,-0.00061315819592252));
#27398=CARTESIAN_POINT('Origin',(-7.7,0.,0.));
#27399=CARTESIAN_POINT('',(-9.12013030787577,-1.95563441709699,-0.00147295684208459));
#27400=CARTESIAN_POINT('',(-9.22186969212424,-1.95583091145133,-0.00139679566445557));
#27401=CARTESIAN_POINT('',(-7.7,-1.954,-2.39295984553393E-16));
#27402=CARTESIAN_POINT('Ctrl Pts',(-9.12013030787577,-1.95563441709699,
-0.00147295684208459));
#27403=CARTESIAN_POINT('Ctrl Pts',(-9.15168162443136,-1.95100144064053,
0.550550385164461));
#27404=CARTESIAN_POINT('Ctrl Pts',(-9.18323294098694,-1.70599712346534,
1.10617250200022));
#27405=CARTESIAN_POINT('Ctrl Pts',(-9.21478425754253,-1.29228238927443,
1.46989630015075));
#27406=CARTESIAN_POINT('Ctrl Pts',(-9.25179142323547,-0.807028162534314,
1.89651516535433));
#27407=CARTESIAN_POINT('Ctrl Pts',(-9.28879858892841,-0.0896720996266766,
2.05913164758619));
#27408=CARTESIAN_POINT('Ctrl Pts',(-9.32580575462135,0.53211317608774,1.88346608003955));
#27409=CARTESIAN_POINT('Ctrl Pts',(-9.3628129203143,1.15389845180216,1.70780051249291));
#27410=CARTESIAN_POINT('Ctrl Pts',(-9.39982008600724,1.68011294032337,1.19385289516776));
#27411=CARTESIAN_POINT('Ctrl Pts',(-9.43682725170018,1.87039332583119,0.5763833043313));
#27412=CARTESIAN_POINT('Ctrl Pts',(-9.47383441739312,2.06067371133901,-0.0410862865051484));
#27413=CARTESIAN_POINT('Ctrl Pts',(-9.51084158308607,1.91501999383345,-0.762077850852902));
#27414=CARTESIAN_POINT('Ctrl Pts',(-9.54784874877901,1.49996361869444,-1.25725814748555));
#27415=CARTESIAN_POINT('Ctrl Pts',(-9.58485591447195,1.08490724355543,-1.7524384441182));
#27416=CARTESIAN_POINT('Ctrl Pts',(-9.62186308016489,0.400448210782955,
-2.02180747303574));
#27417=CARTESIAN_POINT('Ctrl Pts',(-9.65887024585783,-0.240767503031595,
-1.94232332949735));
#27418=CARTESIAN_POINT('Ctrl Pts',(-9.69587741155078,-0.881983216846153,
-1.86283918595894));
#27419=CARTESIAN_POINT('Ctrl Pts',(-9.73288457724372,-1.47995561170279,
-1.43450186996459));
#27420=CARTESIAN_POINT('Ctrl Pts',(-9.76989174293666,-1.76154392327062,
-0.852966536983759));
#27421=CARTESIAN_POINT('Ctrl Pts',(-9.7866379312497,-1.88896602663815,-0.589814792870613));
#27422=CARTESIAN_POINT('Ctrl Pts',(-9.80338411956273,-1.95160306202713,
-0.295293126979237));
#27423=CARTESIAN_POINT('Ctrl Pts',(-9.82013030787577,-1.95092775659677,
-0.000499046442109796));
#27424=CARTESIAN_POINT('Ctrl Pts',(-9.92186969212424,-1.950990226885,-0.00061315819592252));
#27425=CARTESIAN_POINT('Ctrl Pts',(-9.90554051204985,-1.95180076361229,
-0.288043348493711));
#27426=CARTESIAN_POINT('Ctrl Pts',(-9.88921133197546,-1.8923706209308,-0.57515464737431));
#27427=CARTESIAN_POINT('Ctrl Pts',(-9.87288215190107,-1.77101071131092,
-0.833132469350365));
#27428=CARTESIAN_POINT('Ctrl Pts',(-9.83587498620812,-1.49597018488382,
-1.4177930560717));
#27429=CARTESIAN_POINT('Ctrl Pts',(-9.79886782051518,-0.902845282023798,
-1.85281794589588));
#27430=CARTESIAN_POINT('Ctrl Pts',(-9.76186065482224,-0.262562538310644,
-1.93949724530346));
#27431=CARTESIAN_POINT('Ctrl Pts',(-9.7248534891293,0.377720205402501,-2.02617654471103));
#27432=CARTESIAN_POINT('Ctrl Pts',(-9.68784632343636,1.06516078996877,-1.76451025370202));
#27433=CARTESIAN_POINT('Ctrl Pts',(-9.65083915774341,1.48575133088456,-1.27402183412946));
#27434=CARTESIAN_POINT('Ctrl Pts',(-9.61383199205047,1.90634187180036,-0.783533414556894));
#27435=CARTESIAN_POINT('Ctrl Pts',(-9.57682482635753,2.06008236906566,-0.0642228664207834));
#27436=CARTESIAN_POINT('Ctrl Pts',(-9.53981766066459,1.87674751246072,0.555344420640338));
#27437=CARTESIAN_POINT('Ctrl Pts',(-9.50281049497165,1.69341265585578,1.17491170770145));
#27438=CARTESIAN_POINT('Ctrl Pts',(-9.4658033292787,1.17300244538061,1.69473573368758));
#27439=CARTESIAN_POINT('Ctrl Pts',(-9.42879616358576,0.553228929078587,
1.87737220686107));
#27440=CARTESIAN_POINT('Ctrl Pts',(-9.39178899789282,-0.0665445872234321,
2.06000868003456));
#27441=CARTESIAN_POINT('Ctrl Pts',(-9.35478183219989,-0.785681409352301,
1.90545760039541));
#27442=CARTESIAN_POINT('Ctrl Pts',(-9.31777466650694,-1.27569550192533,
1.48431453453482));
#27443=CARTESIAN_POINT('Ctrl Pts',(-9.28580634171271,-1.6989900010259,1.12051368509993));
#27444=CARTESIAN_POINT('Ctrl Pts',(-9.25383801691847,-1.95130805500872,
0.557776003036592));
#27445=CARTESIAN_POINT('Ctrl Pts',(-9.22186969212424,-1.95583091145133,
-0.00139679566445557));
#27446=CARTESIAN_POINT('Origin',(-7.7,0.,0.));
#27447=CARTESIAN_POINT('',(-8.42013030787577,-1.95544987894172,0.00153511913569427));
#27448=CARTESIAN_POINT('',(-8.52186969212424,-1.95524099021,0.00159565242000603));
#27449=CARTESIAN_POINT('',(-7.7,-1.954,-2.39295984553393E-16));
#27450=CARTESIAN_POINT('Ctrl Pts',(-8.42013030787577,-1.95544987894172,
0.00153511913569427));
#27451=CARTESIAN_POINT('Ctrl Pts',(-8.4259647979141,-1.95633055877726,0.103640688502044));
#27452=CARTESIAN_POINT('Ctrl Pts',(-8.43179928795242,-1.94902185525376,
0.205619918324635));
#27453=CARTESIAN_POINT('Ctrl Pts',(-8.43763377799075,-1.93308324972855,
0.306232030402798));
#27454=CARTESIAN_POINT('Ctrl Pts',(-8.47464094368369,-1.83198741929417,
0.944397333271522));
#27455=CARTESIAN_POINT('Ctrl Pts',(-8.51164810937664,-1.38369799135314,
1.5275614869025));
#27456=CARTESIAN_POINT('Ctrl Pts',(-8.54865527506958,-0.792983811495096,
1.78934780898864));
#27457=CARTESIAN_POINT('Ctrl Pts',(-8.58566244076252,-0.202269631637063,
2.05113413107477));
#27458=CARTESIAN_POINT('Ctrl Pts',(-8.62266960645546,0.530869300137978,
1.99154262161609));
#27459=CARTESIAN_POINT('Ctrl Pts',(-8.6596767721484,1.07155108976907,1.63779338405076));
#27460=CARTESIAN_POINT('Ctrl Pts',(-8.69668393784134,1.61223287940017,1.28404414648543));
#27461=CARTESIAN_POINT('Ctrl Pts',(-8.73369110353428,1.96045752688732,0.636137180813462));
#27462=CARTESIAN_POINT('Ctrl Pts',(-8.77069826922723,1.95716359863995,-0.00997772441117081));
#27463=CARTESIAN_POINT('Ctrl Pts',(-8.80770543492017,1.95386967039258,-0.656092629635813));
#27464=CARTESIAN_POINT('Ctrl Pts',(-8.84471260061312,1.59905716641068,-1.30041547441312));
#27465=CARTESIAN_POINT('Ctrl Pts',(-8.88171976630606,1.05479670962828,-1.64863361854084));
#27466=CARTESIAN_POINT('Ctrl Pts',(-8.918726931999,0.510536252845885,-1.99685176266856));
#27467=CARTESIAN_POINT('Ctrl Pts',(-8.95573409769193,-0.22317215673701,
-2.0489652061467));
#27468=CARTESIAN_POINT('Ctrl Pts',(-8.99274126338488,-0.811186500001768,
-1.7811696631822));
#27469=CARTESIAN_POINT('Ctrl Pts',(-9.02974842907782,-1.39920084326652,
-1.5133741202177));
#27470=CARTESIAN_POINT('Ctrl Pts',(-9.06675559477076,-1.84152112021314,
-0.925669590810556));
#27471=CARTESIAN_POINT('Ctrl Pts',(-9.10376276046371,-1.93610506340016,
-0.286506702019341));
#27472=CARTESIAN_POINT('Ctrl Pts',(-9.10921860960106,-1.95004927434369,
-0.192276943264637));
#27473=CARTESIAN_POINT('Ctrl Pts',(-9.11467445873842,-1.95643555072192,
-0.0969287540345871));
#27474=CARTESIAN_POINT('Ctrl Pts',(-9.12013030787577,-1.95563441709699,
-0.00147295684208459));
#27475=CARTESIAN_POINT('Ctrl Pts',(-9.22186969212424,-1.95583091145133,
-0.00139679566445557));
#27476=CARTESIAN_POINT('Ctrl Pts',(-9.21683085122553,-1.95654380317051,
-0.0895334992820675));
#27477=CARTESIAN_POINT('Ctrl Pts',(-9.21179201032682,-1.95110047081772,
-0.177581636934776));
#27478=CARTESIAN_POINT('Ctrl Pts',(-9.20675316942811,-1.93920009935021,
-0.264748230860875));
#27479=CARTESIAN_POINT('Ctrl Pts',(-9.16974600373516,-1.85179924118489,
-0.904932878313924));
#27480=CARTESIAN_POINT('Ctrl Pts',(-9.13273883804223,-1.41610616183707,
-1.49756712113799));
#27481=CARTESIAN_POINT('Ctrl Pts',(-9.09573167234929,-0.831135969245425,
-1.77194854656965));
#27482=CARTESIAN_POINT('Ctrl Pts',(-9.05872450665635,-0.246165776653769,
-2.04632997200132));
#27483=CARTESIAN_POINT('Ctrl Pts',(-9.0217173409634,0.488081529181725,-2.00245858004057));
#27484=CARTESIAN_POINT('Ctrl Pts',(-8.98471017527046,1.03621777307301,-1.66037386688404));
#27485=CARTESIAN_POINT('Ctrl Pts',(-8.94770300957752,1.58435401696429,-1.31828915372751));
#27486=CARTESIAN_POINT('Ctrl Pts',(-8.91069584388458,1.94637919891136,-0.677991119375211));
#27487=CARTESIAN_POINT('Ctrl Pts',(-8.87368867819164,1.95692810179956,-0.0319539582997181));
#27488=CARTESIAN_POINT('Ctrl Pts',(-8.8366815124987,1.96747700468776,0.61408320277577));
#27489=CARTESIAN_POINT('Ctrl Pts',(-8.79967434680575,1.62654962851709,1.26585949057444));
#27490=CARTESIAN_POINT('Ctrl Pts',(-8.76266718111281,1.0898741722973,1.62565769448033));
#27491=CARTESIAN_POINT('Ctrl Pts',(-8.72566001541987,0.553198716077507,
1.98545589838623));
#27492=CARTESIAN_POINT('Ctrl Pts',(-8.68865284972692,-0.179224820191409,
2.05327601839933));
#27493=CARTESIAN_POINT('Ctrl Pts',(-8.65164568403398,-0.772841319532216,
1.79813930102413));
#27494=CARTESIAN_POINT('Ctrl Pts',(-8.61463851834104,-1.36645781887302,
1.54300258364892));
#27495=CARTESIAN_POINT('Ctrl Pts',(-8.5776313526481,-1.82126728128571,0.964909028885417));
#27496=CARTESIAN_POINT('Ctrl Pts',(-8.54062418695516,-1.92952265146001,
0.32791917993094));
#27497=CARTESIAN_POINT('Ctrl Pts',(-8.53437268867819,-1.94780987360863,
0.220314588532923));
#27498=CARTESIAN_POINT('Ctrl Pts',(-8.52812119040122,-1.95620774879912,
0.111029318993031));
#27499=CARTESIAN_POINT('Ctrl Pts',(-8.52186969212424,-1.95524099021,0.00159565242000603));
#27500=CARTESIAN_POINT('Origin',(-7.7,0.,0.));
#27501=CARTESIAN_POINT('',(-7.72013030787577,-1.9508822561445,0.000393506593624193));
#27502=CARTESIAN_POINT('',(-7.82186969212424,-1.95084466165673,0.000275628296667681));
#27503=CARTESIAN_POINT('',(-7.7,-1.954,-2.39295984553393E-16));
#27504=CARTESIAN_POINT('Ctrl Pts',(-7.72013030787577,-1.9508822561445,0.000393506593624193));
#27505=CARTESIAN_POINT('Ctrl Pts',(-7.73725513708977,-1.95142606804339,
0.301870604817531));
#27506=CARTESIAN_POINT('Ctrl Pts',(-7.75437996630378,-1.88579578422546,
0.60312340631659));
#27507=CARTESIAN_POINT('Ctrl Pts',(-7.77150479551779,-1.75275564830829,
0.870882623634832));
#27508=CARTESIAN_POINT('Ctrl Pts',(-7.80851196121073,-1.46525273121817,
1.44951669917947));
#27509=CARTESIAN_POINT('Ctrl Pts',(-7.84551912690368,-0.862944158876693,
1.87173491878606));
#27510=CARTESIAN_POINT('Ctrl Pts',(-7.88252629259662,-0.220951367034791,
1.94467719692271));
#27511=CARTESIAN_POINT('Ctrl Pts',(-7.91953345828957,0.421041424807139,
2.01761947505937));
#27512=CARTESIAN_POINT('Ctrl Pts',(-7.95654062398251,1.10271843614949,1.74128581172607));
#27513=CARTESIAN_POINT('Ctrl Pts',(-7.99354778967545,1.51270445718934,1.24189940495405));
#27514=CARTESIAN_POINT('Ctrl Pts',(-8.03055495536839,1.92269047822918,0.742512998182048));
#27515=CARTESIAN_POINT('Ctrl Pts',(-8.06756212106133,2.06098550896654,0.020073847971333));
#27516=CARTESIAN_POINT('Ctrl Pts',(-8.10456928675427,1.86441939184286,-0.595423578762236));
#27517=CARTESIAN_POINT('Ctrl Pts',(-8.14157645244722,1.66785327471917,-1.21092100549583));
#27518=CARTESIAN_POINT('Ctrl Pts',(-8.17858361814016,1.13642600973442,-1.71947670875229));
#27519=CARTESIAN_POINT('Ctrl Pts',(-8.2155907838331,0.512881995447341,-1.88879352115886));
#27520=CARTESIAN_POINT('Ctrl Pts',(-8.25259794952604,-0.110662018839707,
-2.05811033356542));
#27521=CARTESIAN_POINT('Ctrl Pts',(-8.28960511521899,-0.826322782429062,
-1.88818825512213));
#27522=CARTESIAN_POINT('Ctrl Pts',(-8.32661228091193,-1.30720204775987,
-1.45664398984725));
#27523=CARTESIAN_POINT('Ctrl Pts',(-8.35778495656654,-1.71226666393624,
-1.0931362972117));
#27524=CARTESIAN_POINT('Ctrl Pts',(-8.38895763222116,-1.95074455822154,
-0.543997356792516));
#27525=CARTESIAN_POINT('Ctrl Pts',(-8.42013030787577,-1.95544987894172,
0.00153511913569427));
#27526=CARTESIAN_POINT('Ctrl Pts',(-8.52186969212424,-1.95524099021,0.00159565242000603));
#27527=CARTESIAN_POINT('Ctrl Pts',(-8.49111402470827,-1.95048480148194,
-0.536788156406736));
#27528=CARTESIAN_POINT('Ctrl Pts',(-8.4603583572923,-1.71906965971708,-1.07876372514158));
#27529=CARTESIAN_POINT('Ctrl Pts',(-8.42960268987633,-1.3234761506427,-1.44187361781254));
#27530=CARTESIAN_POINT('Ctrl Pts',(-8.39259552418339,-0.847473001715219,
-1.87879042345607));
#27531=CARTESIAN_POINT('Ctrl Pts',(-8.35558835849045,-0.133765425924392,
-2.05673789159769));
#27532=CARTESIAN_POINT('Ctrl Pts',(-8.31858119279751,0.491640502808977,
-1.89443349502208));
#27533=CARTESIAN_POINT('Ctrl Pts',(-8.28157402710457,1.11704643154235,-1.73212909844647));
#27534=CARTESIAN_POINT('Ctrl Pts',(-8.24456686141163,1.65415071321825,-1.22957283715362));
#27535=CARTESIAN_POINT('Ctrl Pts',(-8.20755969571868,1.85761581171597,-0.616321464113222));
#27536=CARTESIAN_POINT('Ctrl Pts',(-8.17055253002574,2.06108091021368,-0.00307009107281909));
#27537=CARTESIAN_POINT('Ctrl Pts',(-8.1335453643328,1.9309068255332,0.72087639371516));
#27538=CARTESIAN_POINT('Ctrl Pts',(-8.09653819863986,1.52655424397296,1.22483500573424));
#27539=CARTESIAN_POINT('Ctrl Pts',(-8.05953103294691,1.12220166241272,1.72879361775331));
#27540=CARTESIAN_POINT('Ctrl Pts',(-8.02252386725398,0.443670583972736,
2.01276435700351));
#27541=CARTESIAN_POINT('Ctrl Pts',(-7.98551670156103,-0.199100775166,1.94703557553326));
#27542=CARTESIAN_POINT('Ctrl Pts',(-7.94850953586809,-0.841872134304755,
1.88130679406301));
#27543=CARTESIAN_POINT('Ctrl Pts',(-7.91150237017514,-1.44888377414225,
1.46587849187229));
#27544=CARTESIAN_POINT('Ctrl Pts',(-7.8744952044822,-1.74286600014233,0.89050926812229));
#27545=CARTESIAN_POINT('Ctrl Pts',(-7.85695336702955,-1.88221707785663,
0.61777740094752));
#27546=CARTESIAN_POINT('Ctrl Pts',(-7.83941152957689,-1.95123442335438,
0.309108840765172));
#27547=CARTESIAN_POINT('Ctrl Pts',(-7.82186969212424,-1.95084466165673,
0.000275628296667681));
#27548=CARTESIAN_POINT('Origin',(-7.7,0.,0.));
#27549=CARTESIAN_POINT('',(-7.02013030787577,-1.95401264958061,-0.00177430195079181));
#27550=CARTESIAN_POINT('',(-7.12186969212424,-1.95423380238351,-0.00176282217937467));
#27551=CARTESIAN_POINT('',(-7.7,-1.954,-2.39295984553393E-16));
#27552=CARTESIAN_POINT('Ctrl Pts',(-7.02013030787577,-1.95401264958061,
-0.00177430195079181));
#27553=CARTESIAN_POINT('Ctrl Pts',(-7.04854547626546,-1.9494508329156,0.496443956289582));
#27554=CARTESIAN_POINT('Ctrl Pts',(-7.07696064465515,-1.75529612755347,
0.997823441204779));
#27555=CARTESIAN_POINT('Ctrl Pts',(-7.10537581304484,-1.41166222317204,
1.35565433444322));
#27556=CARTESIAN_POINT('Ctrl Pts',(-7.14238297873778,-0.964122491478272,
1.82168384989498));
#27557=CARTESIAN_POINT('Ctrl Pts',(-7.17939014443073,-0.263039573894212,
2.04422953948621));
#27558=CARTESIAN_POINT('Ctrl Pts',(-7.21639731012367,0.371347124525088,
1.92163737992699));
#27559=CARTESIAN_POINT('Ctrl Pts',(-7.25340447581661,1.00573382294441,1.79904522036777));
#27560=CARTESIAN_POINT('Ctrl Pts',(-7.29041164150955,1.57342430219897,1.33131521165807));
#27561=CARTESIAN_POINT('Ctrl Pts',(-7.3274188072025,1.8151099173736,0.732096233208271));
#27562=CARTESIAN_POINT('Ctrl Pts',(-7.36442597289544,2.05679553254821,0.132877254758492));
#27563=CARTESIAN_POINT('Ctrl Pts',(-7.40143313858838,1.97247628364293,-0.597830693431359));
#27564=CARTESIAN_POINT('Ctrl Pts',(-7.43844030428132,1.60066736683049,-1.12625613764794));
#27565=CARTESIAN_POINT('Ctrl Pts',(-7.47544746997426,1.22885845001806,-1.65468158186452));
#27566=CARTESIAN_POINT('Ctrl Pts',(-7.5124546356672,0.569559865298466,-1.98082452210781));
#27567=CARTESIAN_POINT('Ctrl Pts',(-7.54946180136014,-0.0760751553371205,
-1.95570996765015));
#27568=CARTESIAN_POINT('Ctrl Pts',(-7.58646896705309,-0.721710175972735,
-1.93059541319249));
#27569=CARTESIAN_POINT('Ctrl Pts',(-7.62347613274604,-1.35368163252435,
-1.55422336403385));
#27570=CARTESIAN_POINT('Ctrl Pts',(-7.66048329843898,-1.68331872988077,
-0.998512373713166));
#27571=CARTESIAN_POINT('Ctrl Pts',(-7.68036563491791,-1.86041836890632,
-0.699953089647185));
#27572=CARTESIAN_POINT('Ctrl Pts',(-7.70024797139684,-1.9502508775176,-0.349628618162857));
#27573=CARTESIAN_POINT('Ctrl Pts',(-7.72013030787577,-1.9508822561445,0.000393506593624193));
#27574=CARTESIAN_POINT('Ctrl Pts',(-7.82186969212424,-1.95084466165673,
0.000275628296667681));
#27575=CARTESIAN_POINT('Ctrl Pts',(-7.80240436388396,-1.9504121619599,-0.342421644348059));
#27576=CARTESIAN_POINT('Ctrl Pts',(-7.78293903564367,-1.8645168377084,-0.685321657749648));
#27577=CARTESIAN_POINT('Ctrl Pts',(-7.76347370740338,-1.69442477712935,
-0.979547510697657));
#27578=CARTESIAN_POINT('Ctrl Pts',(-7.72646654171044,-1.37104851595361,
-1.53892492045839));
#27579=CARTESIAN_POINT('Ctrl Pts',(-7.68945937601749,-0.743343181439431,
-1.92236959467059));
#27580=CARTESIAN_POINT('Ctrl Pts',(-7.65245221032455,-0.0980308970802916,
-1.95473235873392));
#27581=CARTESIAN_POINT('Ctrl Pts',(-7.61544504463161,0.547281387278848,
-1.98709512279725));
#27582=CARTESIAN_POINT('Ctrl Pts',(-7.57843787893867,1.21020062148296,-1.6683759767117));
#27583=CARTESIAN_POINT('Ctrl Pts',(-7.54143071324573,1.58791973972498,-1.1441588837463));
#27584=CARTESIAN_POINT('Ctrl Pts',(-7.50442354755279,1.965638857967,-0.619941790780907));
#27585=CARTESIAN_POINT('Ctrl Pts',(-7.46741638185984,2.05815786024695,0.10977324906432));
#27586=CARTESIAN_POINT('Ctrl Pts',(-7.4304092161669,1.82321608166587,0.711668300979329));
#27587=CARTESIAN_POINT('Ctrl Pts',(-7.39340205047395,1.58827430308477,1.31356335289435));
#27588=CARTESIAN_POINT('Ctrl Pts',(-7.35639488478102,1.02587174364262,1.78763841687913));
#27589=CARTESIAN_POINT('Ctrl Pts',(-7.31938771908808,0.39290164167109,1.91734633048805));
#27590=CARTESIAN_POINT('Ctrl Pts',(-7.28238055339514,-0.240068460300431,
2.04705424409697));
#27591=CARTESIAN_POINT('Ctrl Pts',(-7.24537338770219,-0.943606104801338,
1.83239500733005));
#27592=CARTESIAN_POINT('Ctrl Pts',(-7.20836622200925,-1.39635062099231,
1.37142028361776));
#27593=CARTESIAN_POINT('Ctrl Pts',(-7.17953404538091,-1.74908257476143,
1.01227619877891));
#27594=CARTESIAN_POINT('Ctrl Pts',(-7.15070186875258,-1.94958502072792,
0.503620500146864));
#27595=CARTESIAN_POINT('Ctrl Pts',(-7.12186969212424,-1.95423380238351,
-0.00176282217937467));
#27596=CARTESIAN_POINT('Origin',(-7.7,0.,0.));
#27597=CARTESIAN_POINT('',(-6.32013030787576,-1.95674715409565,0.000835936956466929));
#27598=CARTESIAN_POINT('',(-6.42186969212424,-1.95661254207068,0.000950563181825557));
#27599=CARTESIAN_POINT('',(-7.7,-1.954,-2.39295984553393E-16));
#27600=CARTESIAN_POINT('Ctrl Pts',(-6.32013030787576,-1.95674715409565,
0.000835936956466929));
#27601=CARTESIAN_POINT('Ctrl Pts',(-6.3228286497482,-1.95700108945633,0.0479758079941679));
#27602=CARTESIAN_POINT('Ctrl Pts',(-6.32552699162063,-1.95544487187201,
0.0950986300560049));
#27603=CARTESIAN_POINT('Ctrl Pts',(-6.32822533349306,-1.95202472787979,
0.142085778920809));
#27604=CARTESIAN_POINT('Ctrl Pts',(-6.365232499186,-1.9051182047639,0.78650419796693));
#27605=CARTESIAN_POINT('Ctrl Pts',(-6.40223966487895,-1.50761607859282,
1.40540314042301));
#27606=CARTESIAN_POINT('Ctrl Pts',(-6.43924683057189,-0.941088661808038,
1.71608305085799));
#27607=CARTESIAN_POINT('Ctrl Pts',(-6.47625399626483,-0.374561245023235,
2.02676296129299));
#27608=CARTESIAN_POINT('Ctrl Pts',(-6.51326116195777,0.360991462375277,
2.02922383970686));
#27609=CARTESIAN_POINT('Ctrl Pts',(-6.55026832765071,0.929585006201032,
1.72234161044549));
#27610=CARTESIAN_POINT('Ctrl Pts',(-6.58727549334365,1.49817855002677,1.41545938118412));
#27611=CARTESIAN_POINT('Ctrl Pts',(-6.6242826590366,1.89981293027976,0.799234044247542));
#27612=CARTESIAN_POINT('Ctrl Pts',(-6.66128982472954,1.95103031086682,0.155143910304678));
#27613=CARTESIAN_POINT('Ctrl Pts',(-6.69829699042249,2.00224769145389,-0.488946223638195));
#27614=CARTESIAN_POINT('Ctrl Pts',(-6.73530415611543,1.70304807237501,-1.16090115458735));
#27615=CARTESIAN_POINT('Ctrl Pts',(-6.77231132180837,1.19009932215664,-1.55378650728729));
#27616=CARTESIAN_POINT('Ctrl Pts',(-6.80931848750131,0.677150571938273,
-1.94667185998723));
#27617=CARTESIAN_POINT('Ctrl Pts',(-6.84632565319425,-0.0495473094195792,
-2.06048763443796));
#27618=CARTESIAN_POINT('Ctrl Pts',(-6.88333281888719,-0.658054559381064,
-1.84324526412073));
#27619=CARTESIAN_POINT('Ctrl Pts',(-6.92033998458013,-1.26656180934255,
-1.62600289380351));
#27620=CARTESIAN_POINT('Ctrl Pts',(-6.95734715027308,-1.75687842790767,
-1.07770237871833));
#27621=CARTESIAN_POINT('Ctrl Pts',(-6.99435431596602,-1.90503846428849,
-0.448795450519591));
#27622=CARTESIAN_POINT('Ctrl Pts',(-7.00294631326927,-1.93943695466724,
-0.302781387299679));
#27623=CARTESIAN_POINT('Ctrl Pts',(-7.01153831057252,-1.95539202259527,
-0.152422359795286));
#27624=CARTESIAN_POINT('Ctrl Pts',(-7.02013030787577,-1.95401264958061,
-0.00177430195079181));
#27625=CARTESIAN_POINT('Ctrl Pts',(-7.12186969212424,-1.95423380238351,
-0.00176282217937467));
#27626=CARTESIAN_POINT('Ctrl Pts',(-7.11369470305964,-1.95555190402003,
-0.145057696746382));
#27627=CARTESIAN_POINT('Ctrl Pts',(-7.10551971399503,-1.94112469613282,
-0.288089494398315));
#27628=CARTESIAN_POINT('Ctrl Pts',(-7.09734472493042,-1.9099577897608,-0.427375587037744));
#27629=CARTESIAN_POINT('Ctrl Pts',(-7.06033755923749,-1.76886905445728,
-1.05790652332323));
#27630=CARTESIAN_POINT('Ctrl Pts',(-7.02333039354454,-1.28474019596922,
-1.61167818523655));
#27631=CARTESIAN_POINT('Ctrl Pts',(-6.9863232278516,-0.678710731069402,
-1.83573974043029));
#27632=CARTESIAN_POINT('Ctrl Pts',(-6.94931606215865,-0.0726812661695574,
-2.05980129562404));
#27633=CARTESIAN_POINT('Ctrl Pts',(-6.91230889646571,0.655248805142062,
-1.95415274409816));
#27634=CARTESIAN_POINT('Ctrl Pts',(-6.87530173077277,1.17257688279952,-1.56705204284606));
#27635=CARTESIAN_POINT('Ctrl Pts',(-6.83829456507983,1.68990496045699,-1.17995134159395));
#27636=CARTESIAN_POINT('Ctrl Pts',(-6.80128739938689,1.99663104446028,-0.511398490615602));
#27637=CARTESIAN_POINT('Ctrl Pts',(-6.76428023369395,1.95264934105456,0.133226130856597));
#27638=CARTESIAN_POINT('Ctrl Pts',(-6.72727306800101,1.90866763764884,0.777850752328768));
#27639=CARTESIAN_POINT('Ctrl Pts',(-6.69026590230807,1.51397814683413,1.3985471442948));
#27640=CARTESIAN_POINT('Ctrl Pts',(-6.65325873661513,0.948866430488816,
1.71179471554134));
#27641=CARTESIAN_POINT('Ctrl Pts',(-6.61625157092218,0.383754714143482,
2.02504228678789));
#27642=CARTESIAN_POINT('Ctrl Pts',(-6.57924440522924,-0.351779227732472,
2.03084103731494));
#27643=CARTESIAN_POINT('Ctrl Pts',(-6.54223723953629,-0.921759512634525,
1.72654222419598));
#27644=CARTESIAN_POINT('Ctrl Pts',(-6.50523007384335,-1.49173979753657,
1.42224341107702));
#27645=CARTESIAN_POINT('Ctrl Pts',(-6.46822290815041,-1.89616642546472,
0.807847034312071));
#27646=CARTESIAN_POINT('Ctrl Pts',(-6.43121574245747,-1.95030612241134,
0.16399597540392));
#27647=CARTESIAN_POINT('Ctrl Pts',(-6.4281003923464,-1.95486372923526,0.109795081324937));
#27648=CARTESIAN_POINT('Ctrl Pts',(-6.42498504223532,-1.9569389689582,0.0553854516995903));
#27649=CARTESIAN_POINT('Ctrl Pts',(-6.42186969212424,-1.95661254207068,
0.000950563181825557));
#27650=CARTESIAN_POINT('Origin',(-7.7,0.,0.));
#27651=CARTESIAN_POINT('',(-5.62013030787577,-1.95157062279887,0.00118915835141939));
#27652=CARTESIAN_POINT('',(-5.72186969212424,-1.95144011146387,0.00109661375529725));
#27653=CARTESIAN_POINT('',(-7.7,-1.954,-2.39295984553393E-16));
#27654=CARTESIAN_POINT('Ctrl Pts',(-5.62013030787577,-1.95157062279887,
0.00118915835141939));
#27655=CARTESIAN_POINT('Ctrl Pts',(-5.63411898892388,-1.95294121534163,
0.247238073111425));
#27656=CARTESIAN_POINT('Ctrl Pts',(-5.648107669972,-1.9098072184107,0.492824110420985));
#27657=CARTESIAN_POINT('Ctrl Pts',(-5.66209635102011,-1.8199678581088,0.719934651393151));
#27658=CARTESIAN_POINT('Ctrl Pts',(-5.69910351671305,-1.58229712410575,
1.32075737309663));
#27659=CARTESIAN_POINT('Ctrl Pts',(-5.73611068240599,-1.01774901009749,
1.79227541967969));
#27660=CARTESIAN_POINT('Ctrl Pts',(-5.77311784809893,-0.384196797004847,
1.9191096185463));
#27661=CARTESIAN_POINT('Ctrl Pts',(-5.81012501379187,0.249355416087819,
2.04594381741292));
#27662=CARTESIAN_POINT('Ctrl Pts',(-5.84713217948482,0.951911728264895,
1.82809416856304));
#27663=CARTESIAN_POINT('Ctrl Pts',(-5.88413934517776,1.40255971991618,1.36506964616989));
#27664=CARTESIAN_POINT('Ctrl Pts',(-5.92114651087071,1.85320771156745,0.902045123776732));
#27665=CARTESIAN_POINT('Ctrl Pts',(-5.95815367656364,2.05194738269297,0.1938457278403));
#27666=CARTESIAN_POINT('Ctrl Pts',(-5.99516084225658,1.90799878067116,-0.436038484291347));
#27667=CARTESIAN_POINT('Ctrl Pts',(-6.03216800794953,1.76405017864935,-1.065922696423));
#27668=CARTESIAN_POINT('Ctrl Pts',(-6.06917517364247,1.27741330348022,-1.61749172474984));
#27669=CARTESIAN_POINT('Ctrl Pts',(-6.10618233933541,0.670373279324294,
-1.83880085196677));
#27670=CARTESIAN_POINT('Ctrl Pts',(-6.14318950502836,0.0633332551683667,
-2.0601099791837));
#27671=CARTESIAN_POINT('Ctrl Pts',(-6.1801966707213,-0.664109917974376,
-1.95115920529068));
#27672=CARTESIAN_POINT('Ctrl Pts',(-6.21720383641424,-1.17967604451539,
-1.56171487052607));
#27673=CARTESIAN_POINT('Ctrl Pts',(-6.25151266023475,-1.65765016309781,
-1.20066649464673));
#27674=CARTESIAN_POINT('Ctrl Pts',(-6.28582148405525,-1.95351842179887,
-0.598537162085356));
#27675=CARTESIAN_POINT('Ctrl Pts',(-6.32013030787576,-1.95674715409565,
0.000835936956466929));
#27676=CARTESIAN_POINT('Ctrl Pts',(-6.42186969212424,-1.95661254207068,
0.000950563181825557));
#27677=CARTESIAN_POINT('Ctrl Pts',(-6.38797787654238,-1.95306135216312,
-0.591245221267486));
#27678=CARTESIAN_POINT('Ctrl Pts',(-6.35408606096051,-1.6652678890792,-1.1864304485344));
#27679=CARTESIAN_POINT('Ctrl Pts',(-6.32019424537865,-1.19713802583512,
-1.54836985186468));
#27680=CARTESIAN_POINT('Ctrl Pts',(-6.2831870796857,-0.685977466347171,
-1.94357887917377));
#27681=CARTESIAN_POINT('Ctrl Pts',(-6.24617991399276,0.0401964185938104,
-2.06069119274061));
#27682=CARTESIAN_POINT('Ctrl Pts',(-6.20917274829982,0.649683216600975,
-1.84621243878673));
#27683=CARTESIAN_POINT('Ctrl Pts',(-6.17216558260688,1.25917001460814,-1.63173368483286));
#27684=CARTESIAN_POINT('Ctrl Pts',(-6.13515841691393,1.75196972568149,-1.08566386335827));
#27685=CARTESIAN_POINT('Ctrl Pts',(-6.09815125122099,1.90298217646455,-0.457435773767298));
#27686=CARTESIAN_POINT('Ctrl Pts',(-6.06114408552805,2.05399462724761,0.170792315823676));
#27687=CARTESIAN_POINT('Ctrl Pts',(-6.02413691983511,1.86321981774039,0.881178673531042));
#27688=CARTESIAN_POINT('Ctrl Pts',(-5.98712975414217,1.41779952527589,1.34923428550837));
#27689=CARTESIAN_POINT('Ctrl Pts',(-5.95012258844923,0.972379232811401,
1.81728989748569));
#27690=CARTESIAN_POINT('Ctrl Pts',(-5.91311542275628,0.272313457389638,
2.04301476373299));
#27691=CARTESIAN_POINT('Ctrl Pts',(-5.87610825706334,-0.362623004317677,
1.92330268231588));
#27692=CARTESIAN_POINT('Ctrl Pts',(-5.8391010913704,-0.997559466024982,
1.80359060089877));
#27693=CARTESIAN_POINT('Ctrl Pts',(-5.80209392567746,-1.56736661401784,
1.33844157181727));
#27694=CARTESIAN_POINT('Ctrl Pts',(-5.76508675998452,-1.81176895520886,
0.740325539209087));
#27695=CARTESIAN_POINT('Ctrl Pts',(-5.75068107069776,-1.90690685951008,
0.507498367447963));
#27696=CARTESIAN_POINT('Ctrl Pts',(-5.736275381411,-1.9527364216002,0.254522807047113));
#27697=CARTESIAN_POINT('Ctrl Pts',(-5.72186969212424,-1.95144011146387,
0.00109661375529725));
#27698=CARTESIAN_POINT('Origin',(-7.7,0.,0.));
#27699=CARTESIAN_POINT('',(-4.92013030787577,-1.95245193048433,-0.00158706406638287));
#27700=CARTESIAN_POINT('',(-5.02186969212424,-1.95264185663859,-0.00163836777318162));
#27701=CARTESIAN_POINT('',(-7.7,-1.954,-2.39295984553393E-16));
#27702=CARTESIAN_POINT('Ctrl Pts',(-4.92013030787577,-1.95245193048433,
-0.00158706406638287));
#27703=CARTESIAN_POINT('Ctrl Pts',(-4.94540932809956,-1.94904718301888,
0.442544332783492));
#27704=CARTESIAN_POINT('Ctrl Pts',(-4.97068834832336,-1.79874664837135,
0.88876049721347));
#27705=CARTESIAN_POINT('Ctrl Pts',(-4.99596736854716,-1.52098034279809,
1.23174985433226));
#27706=CARTESIAN_POINT('Ctrl Pts',(-5.0329745342401,-1.11434497468405,1.73386836436301));
#27707=CARTESIAN_POINT('Ctrl Pts',(-5.06998169993304,-0.4345322164979,2.01475705244277));
#27708=CARTESIAN_POINT('Ctrl Pts',(-5.10698886562598,0.207934272190149,
1.94611208445826));
#27709=CARTESIAN_POINT('Ctrl Pts',(-5.14399603131892,0.850400760878179,
1.87746711647375));
#27710=CARTESIAN_POINT('Ctrl Pts',(-5.18100319701187,1.45552098006812,1.45928849242499));
#27711=CARTESIAN_POINT('Ctrl Pts',(-5.21801036270481,1.74688919497478,0.882591098587607));
#27712=CARTESIAN_POINT('Ctrl Pts',(-5.25501752839775,2.03825740988146,0.305893704750204));
#27713=CARTESIAN_POINT('Ctrl Pts',(-5.29202469409069,2.01587362050484,-0.42932245887581));
#27714=CARTESIAN_POINT('Ctrl Pts',(-5.32903185978363,1.68996225424583,-0.98722666396835));
#27715=CARTESIAN_POINT('Ctrl Pts',(-5.36603902547657,1.36405088798683,-1.54513086906087));
#27716=CARTESIAN_POINT('Ctrl Pts',(-5.40304619116952,0.734611944845429,
-1.92572311561991));
#27717=CARTESIAN_POINT('Ctrl Pts',(-5.44005335686246,0.0891594229728106,
-1.95515715586264));
#27718=CARTESIAN_POINT('Ctrl Pts',(-5.4770605225554,-0.556293098899808,
-1.98459119610536));
#27719=CARTESIAN_POINT('Ctrl Pts',(-5.51406768824834,-1.21775919950366,
-1.66286703003176));
#27720=CARTESIAN_POINT('Ctrl Pts',(-5.55107485394128,-1.59309557280667,
-1.13694124858302));
#27721=CARTESIAN_POINT('Ctrl Pts',(-5.57409333858611,-1.82655507676345,
-0.809815020515635));
#27722=CARTESIAN_POINT('Ctrl Pts',(-5.59711182323094,-1.94931530199406,
-0.40368626534284));
#27723=CARTESIAN_POINT('Ctrl Pts',(-5.62013030787577,-1.95157062279887,
0.00118915835141939));
#27724=CARTESIAN_POINT('Ctrl Pts',(-5.72186969212424,-1.95144011146387,
0.00109661375529725));
#27725=CARTESIAN_POINT('Ctrl Pts',(-5.69926821571806,-1.94940629535287,
-0.396510610333469));
#27726=CARTESIAN_POINT('Ctrl Pts',(-5.67666673931187,-1.8313706242534,-0.795227081822891));
#27727=CARTESIAN_POINT('Ctrl Pts',(-5.65406526290569,-1.60576172018975,
-1.11898076347947));
#27728=CARTESIAN_POINT('Ctrl Pts',(-5.61705809721275,-1.23635460959044,
-1.64908799742492));
#27729=CARTESIAN_POINT('Ctrl Pts',(-5.58005093151981,-0.578542854002666,
-1.97821942918092));
#27730=CARTESIAN_POINT('Ctrl Pts',(-5.54304376582687,0.0671994657422203,
-1.95603499019516));
#27731=CARTESIAN_POINT('Ctrl Pts',(-5.50603660013393,0.712941785487116,
-1.9338505512094));
#27732=CARTESIAN_POINT('Ctrl Pts',(-5.46902943444098,1.34661466938912,-1.56035024148186));
#27733=CARTESIAN_POINT('Ctrl Pts',(-5.43202226874804,1.6787701473856,-1.00614086653448));
#27734=CARTESIAN_POINT('Ctrl Pts',(-5.3950151030551,2.01092562538208,-0.451931491587115));
#27735=CARTESIAN_POINT('Ctrl Pts',(-5.35800793736216,2.04156369747304,0.282986948580081));
#27736=CARTESIAN_POINT('Ctrl Pts',(-5.32100077166922,1.75668955971682,0.862919719235671));
#27737=CARTESIAN_POINT('Ctrl Pts',(-5.28399360597628,1.4718154219606,1.44285248989126));
#27738=CARTESIAN_POINT('Ctrl Pts',(-5.24698644028333,0.871429074357163,
1.86779959103526));
#27739=CARTESIAN_POINT('Ctrl Pts',(-5.20997927459039,0.229773922269001,
1.94365444349271));
#27740=CARTESIAN_POINT('Ctrl Pts',(-5.17297210889745,-0.411881229819169,
2.01950929595016));
#27741=CARTESIAN_POINT('Ctrl Pts',(-5.13596494320451,-1.09480518639206,
1.74627189972109));
#27742=CARTESIAN_POINT('Ctrl Pts',(-5.09895777751157,-1.50705316022771,
1.24875114546955));
#27743=CARTESIAN_POINT('Ctrl Pts',(-5.07326174904912,-1.79329868784144,
0.903296225523015));
#27744=CARTESIAN_POINT('Ctrl Pts',(-5.04756572058668,-1.94904434446389,
0.449708515251178));
#27745=CARTESIAN_POINT('Ctrl Pts',(-5.02186969212424,-1.95264185663859,
-0.00163836777318162));
#27746=CARTESIAN_POINT('Origin',(-7.7,0.,0.));
#27747=CARTESIAN_POINT('',(-4.22013030787576,-1.95717603808304,-0.000142023995625407));
#27748=CARTESIAN_POINT('',(-4.32186969212423,-1.95718893672642,-6.75583561184207E-6));
#27749=CARTESIAN_POINT('',(-7.7,-1.954,-2.39295984553393E-16));
#27750=CARTESIAN_POINT('Ctrl Pts',(-4.22013030787576,-1.95717603808304,
-0.000142023995625407));
#27751=CARTESIAN_POINT('Ctrl Pts',(-4.25669966727524,-1.95650647305912,
0.638348883812147));
#27752=CARTESIAN_POINT('Ctrl Pts',(-4.29326902667472,-1.6144202457463,1.27745536120794));
#27753=CARTESIAN_POINT('Ctrl Pts',(-4.3298383860742,-1.08248584150121,1.63058679921527));
#27754=CARTESIAN_POINT('Ctrl Pts',(-4.36684555176715,-0.544183148784234,
1.98794590673933));
#27755=CARTESIAN_POINT('Ctrl Pts',(-4.40385271746009,0.188540634495529,
2.05244163295488));
#27756=CARTESIAN_POINT('Ctrl Pts',(-4.44085988315303,0.780993245066536,
1.79461373503777));
#27757=CARTESIAN_POINT('Ctrl Pts',(-4.47786704884597,1.37344585563752,1.53678583712066));
#27758=CARTESIAN_POINT('Ctrl Pts',(-4.51487421453891,1.82562729349976,0.956634315070912));
#27759=CARTESIAN_POINT('Ctrl Pts',(-4.55188138023185,1.93099092771133,0.319159746713509));
#27760=CARTESIAN_POINT('Ctrl Pts',(-4.5888885459248,2.03635456192291,-0.318314821643903));
#27761=CARTESIAN_POINT('Ctrl Pts',(-4.62589571161774,1.79490039248382,-1.01311243630897));
#27762=CARTESIAN_POINT('Ctrl Pts',(-4.66290287731068,1.31691942439483,-1.44786468168724));
#27763=CARTESIAN_POINT('Ctrl Pts',(-4.69991004300362,0.838938456305839,
-1.88261692706552));
#27764=CARTESIAN_POINT('Ctrl Pts',(-4.73691720869656,0.124430689566952,
-2.057323803157));
#27765=CARTESIAN_POINT('Ctrl Pts',(-4.77392437438951,-0.5002322921065,-1.89218301460498));
#27766=CARTESIAN_POINT('Ctrl Pts',(-4.81093154008245,-1.12489527377994,
-1.72704222605298));
#27767=CARTESIAN_POINT('Ctrl Pts',(-4.84793870577539,-1.65971347038795,
-1.22205377285749));
#27768=CARTESIAN_POINT('Ctrl Pts',(-4.88494587146833,-1.860393579671,-0.607885380268879));
#27769=CARTESIAN_POINT('Ctrl Pts',(-4.89667401693748,-1.92399222253827,
-0.413245879622015));
#27770=CARTESIAN_POINT('Ctrl Pts',(-4.90840216240662,-1.95403155553336,
-0.207640842399378));
#27771=CARTESIAN_POINT('Ctrl Pts',(-4.92013030787577,-1.95245193048433,
-0.00158706406638287));
#27772=CARTESIAN_POINT('Ctrl Pts',(-5.02186969212424,-1.95264185663859,
-0.00163836777318162));
#27773=CARTESIAN_POINT('Ctrl Pts',(-5.01055855489374,-1.9542254458674,-0.200316795449617));
#27774=CARTESIAN_POINT('Ctrl Pts',(-4.99924741766324,-1.92632769683691,
-0.398561024034741));
#27775=CARTESIAN_POINT('Ctrl Pts',(-4.98793628043274,-1.86710213185347,
-0.586956795933102));
#27776=CARTESIAN_POINT('Ctrl Pts',(-4.9509291147398,-1.67333113854519,-1.20333987081021));
#27777=CARTESIAN_POINT('Ctrl Pts',(-4.91392194904685,-1.14421716083023,
-1.71430190829039));
#27778=CARTESIAN_POINT('Ctrl Pts',(-4.87691478335391,-0.521447938032845,
-1.88644657994472));
#27779=CARTESIAN_POINT('Ctrl Pts',(-4.83990761766097,0.10132128476453,-2.05859125159905));
#27780=CARTESIAN_POINT('Ctrl Pts',(-4.80290045196803,0.817745752644318,
-1.89191855742752));
#27781=CARTESIAN_POINT('Ctrl Pts',(-4.76589328627509,1.30057837456157,-1.46256095349446));
#27782=CARTESIAN_POINT('Ctrl Pts',(-4.72888612058215,1.78341099647882,-1.0332033495614));
#27783=CARTESIAN_POINT('Ctrl Pts',(-4.6918789548892,2.03265177243352,-0.341160835866783));
#27784=CARTESIAN_POINT('Ctrl Pts',(-4.65487178919626,1.93445294518429,0.297456642103794));
#27785=CARTESIAN_POINT('Ctrl Pts',(-4.61786462350332,1.83625411793506,0.936074120074369));
#27786=CARTESIAN_POINT('Ctrl Pts',(-4.58085745781037,1.3906156874819,1.52126656232092));
#27787=CARTESIAN_POINT('Ctrl Pts',(-4.54385029211743,0.801095581508699,
1.785730808479));
#27788=CARTESIAN_POINT('Ctrl Pts',(-4.50684312642449,0.211575475535495,
2.05019505463709));
#27789=CARTESIAN_POINT('Ctrl Pts',(-4.46983596073155,-0.521826305957753,
1.99393110470671));
#27790=CARTESIAN_POINT('Ctrl Pts',(-4.43282879503861,-1.06410780488448,
1.6426391054178));
#27791=CARTESIAN_POINT('Ctrl Pts',(-4.39584242740049,-1.60608454120294,
1.2915445324954));
#27792=CARTESIAN_POINT('Ctrl Pts',(-4.35885605976236,-1.95715575407421,
0.645753429000468));
#27793=CARTESIAN_POINT('Ctrl Pts',(-4.32186969212423,-1.95718893672642,
-6.75583561184207E-6));
#27794=CARTESIAN_POINT('Origin',(-7.7,0.,0.));
#27795=CARTESIAN_POINT('',(-3.52013030787576,-1.95285875419799,0.00168591294888436));
#27796=CARTESIAN_POINT('',(-3.62186969212424,-1.95266119647961,0.00164306867381859));
#27797=CARTESIAN_POINT('',(-7.7,-1.954,-2.39295984553393E-16));
#27798=CARTESIAN_POINT('Ctrl Pts',(-3.52013030787576,-1.95285875419799,
0.00168591294888436));
#27799=CARTESIAN_POINT('Ctrl Pts',(-3.53098284075798,-1.95443499456628,
0.192255467216998));
#27800=CARTESIAN_POINT('Ctrl Pts',(-3.5418353736402,-1.9287959273972,0.382409993933235));
#27801=CARTESIAN_POINT('Ctrl Pts',(-3.55268790652243,-1.87420812867872,
0.56385529812026));
#27802=CARTESIAN_POINT('Ctrl Pts',(-3.58969507221537,-1.6880635913701,1.18258426297381));
#27803=CARTESIAN_POINT('Ctrl Pts',(-3.62670223790831,-1.1652997890823,1.70004136099891));
#27804=CARTESIAN_POINT('Ctrl Pts',(-3.66370940360125,-0.544703839327083,
1.87986346159656));
#27805=CARTESIAN_POINT('Ctrl Pts',(-3.70071656929419,0.0758921104281432,
2.05968556219421));
#27806=CARTESIAN_POINT('Ctrl Pts',(-3.73772373498713,0.794320207650795,
1.9018726653644));
#27807=CARTESIAN_POINT('Ctrl Pts',(-3.77473090068007,1.28241814705543,1.47851026473626));
#27808=CARTESIAN_POINT('Ctrl Pts',(-3.81173806637301,1.77051608646007,1.05514786410812));
#27809=CARTESIAN_POINT('Ctrl Pts',(-3.84874523206596,2.02828386804669,0.366235959681632));
#27810=CARTESIAN_POINT('Ctrl Pts',(-3.8857523977589,1.93797878414602,-0.27354549717586));
#27811=CARTESIAN_POINT('Ctrl Pts',(-3.92275956345184,1.84767370024536,-0.913326954033334));
#27812=CARTESIAN_POINT('Ctrl Pts',(-3.95976672914478,1.40929575085742,-1.50397796332182));
#27813=CARTESIAN_POINT('Ctrl Pts',(-3.99677389483772,0.823086434070165,
-1.77570201015686));
#27814=CARTESIAN_POINT('Ctrl Pts',(-4.03378106053066,0.236877117282891,
-2.04742605699191));
#27815=CARTESIAN_POINT('Ctrl Pts',(-4.07078822622361,-0.497163566903715,
-2.0002231413735));
#27816=CARTESIAN_POINT('Ctrl Pts',(-4.10779539191655,-1.04374182356972,
-1.65565452693409));
#27817=CARTESIAN_POINT('Ctrl Pts',(-4.14480255760949,-1.59032008023574,
-1.31108591249467));
#27818=CARTESIAN_POINT('Ctrl Pts',(-4.18180972330244,-1.94943590938115,
-0.669151599234243));
#27819=CARTESIAN_POINT('Ctrl Pts',(-4.21881688899538,-1.95705302287675,
-0.0230731981877537));
#27820=CARTESIAN_POINT('Ctrl Pts',(-4.21925469528884,-1.95714313570123,
-0.0154298895270845));
#27821=CARTESIAN_POINT('Ctrl Pts',(-4.2196925015823,-1.95718405407747,-0.00778600087535643));
#27822=CARTESIAN_POINT('Ctrl Pts',(-4.22013030787576,-1.95717603808304,
-0.000142023995625407));
#27823=CARTESIAN_POINT('Ctrl Pts',(-4.32186969212423,-1.95718893672642,
-6.75583561184207E-6));
#27824=CARTESIAN_POINT('Ctrl Pts',(-4.28484172837648,-1.95722215669696,
-0.646493184235486));
#27825=CARTESIAN_POINT('Ctrl Pts',(-4.24781376462872,-1.60524684540183,
-1.29294852331618));
#27826=CARTESIAN_POINT('Ctrl Pts',(-4.21078580088096,-1.06226722191928,
-1.64382997913402));
#27827=CARTESIAN_POINT('Ctrl Pts',(-4.17377863518802,-0.519592581990526,
-1.99451435007294));
#27828=CARTESIAN_POINT('Ctrl Pts',(-4.13677146949508,0.213871760525216,
-2.04995678343623));
#27829=CARTESIAN_POINT('Ctrl Pts',(-4.09976430380213,0.803095271029007,
-1.78483238336676));
#27830=CARTESIAN_POINT('Ctrl Pts',(-4.06275713810919,1.3923187815328,-1.51970798329728));
#27831=CARTESIAN_POINT('Ctrl Pts',(-4.02574997241625,1.83730146002465,-0.93401674979504));
#27832=CARTESIAN_POINT('Ctrl Pts',(-3.98874280672331,1.93478491203242,-0.295289680204818));
#27833=CARTESIAN_POINT('Ctrl Pts',(-3.95173564103036,2.03226836404019,0.343437389385403));
#27834=CARTESIAN_POINT('Ctrl Pts',(-3.91472847533742,1.7822525895639,1.03520029506359));
#27835=CARTESIAN_POINT('Ctrl Pts',(-3.87772130964448,1.29893934828762,1.46401681019524));
#27836=CARTESIAN_POINT('Ctrl Pts',(-3.84071414395154,0.815626107011349,
1.89283332532687));
#27837=CARTESIAN_POINT('Ctrl Pts',(-3.8037069782586,0.0990153989350884,
2.05870344991196));
#27838=CARTESIAN_POINT('Ctrl Pts',(-3.76669981256566,-0.523560614431006,
1.8858613241912));
#27839=CARTESIAN_POINT('Ctrl Pts',(-3.72969264687271,-1.14613662779711,
1.71301919847044));
#27840=CARTESIAN_POINT('Ctrl Pts',(-3.69268548117977,-1.67467794645305,
1.20146482244383));
#27841=CARTESIAN_POINT('Ctrl Pts',(-3.65567831548683,-1.86775840925908,
0.584865091884778));
#27842=CARTESIAN_POINT('Ctrl Pts',(-3.64440877436597,-1.92655589278652,
0.397096158800172));
#27843=CARTESIAN_POINT('Ctrl Pts',(-3.6331392332451,-1.95424461873575,0.199585908921427));
#27844=CARTESIAN_POINT('Ctrl Pts',(-3.62186969212424,-1.95266119647961,
0.00164306867381859));
#27845=CARTESIAN_POINT('Origin',(-7.7,0.,0.));
#27846=CARTESIAN_POINT('',(-2.82013030787576,-1.95130973680355,-0.000989162390181431));
#27847=CARTESIAN_POINT('',(-2.92186969212423,-1.95142771007674,-0.00108710473741568));
#27848=CARTESIAN_POINT('',(-7.7,-1.954,-2.39295984553393E-16));
#27849=CARTESIAN_POINT('Ctrl Pts',(-2.82013030787576,-1.95130973680355,
-0.000989162390181431));
#27850=CARTESIAN_POINT('Ctrl Pts',(-2.84227317993367,-1.94951961830664,
0.388615496325764));
#27851=CARTESIAN_POINT('Ctrl Pts',(-2.86441605199157,-1.83655492906094,
0.779176241682102));
#27852=CARTESIAN_POINT('Ctrl Pts',(-2.88655892404947,-1.61945757610167,
1.09906599712299));
#27853=CARTESIAN_POINT('Ctrl Pts',(-2.92356608974241,-1.25662489154953,
1.6336946194679));
#27854=CARTESIAN_POINT('Ctrl Pts',(-2.96057325543535,-0.602927702481477,
1.97092425351893));
#27855=CARTESIAN_POINT('Ctrl Pts',(-2.99758042112829,0.0430393547874399,
1.95671574855002));
#27856=CARTESIAN_POINT('Ctrl Pts',(-3.03458758682123,0.689006412056357,
1.9425072435811));
#27857=CARTESIAN_POINT('Ctrl Pts',(-3.07159475251418,1.32724333752614,1.57686059959224));
#27858=CARTESIAN_POINT('Ctrl Pts',(-3.10860191820712,1.66621740628167,1.02679523855085));
#27859=CARTESIAN_POINT('Ctrl Pts',(-3.14560908390006,2.00519147503719,0.476729877509469));
#27860=CARTESIAN_POINT('Ctrl Pts',(-3.18261624959301,2.04490268707848,-0.257754200584423));
#27861=CARTESIAN_POINT('Ctrl Pts',(-3.21962341528595,1.76721182581842,-0.841160668068887));
#27862=CARTESIAN_POINT('Ctrl Pts',(-3.25663058097889,1.48952096455835,-1.42456713555338));
#27863=CARTESIAN_POINT('Ctrl Pts',(-3.29363774667183,0.894428029996892,
-1.85689599242844));
#27864=CARTESIAN_POINT('Ctrl Pts',(-3.33064491236477,0.253758511702538,
-1.9406688343316));
#27865=CARTESIAN_POINT('Ctrl Pts',(-3.36765207805771,-0.386911006591771,
-2.02444167623475));
#27866=CARTESIAN_POINT('Ctrl Pts',(-3.40465924375065,-1.07315710861897,
-1.75965850316607));
#27867=CARTESIAN_POINT('Ctrl Pts',(-3.4416664094436,-1.49151752346787,-1.26726650079074));
#27868=CARTESIAN_POINT('Ctrl Pts',(-3.46782104225432,-1.78719169434882,
-0.919270868595652));
#27869=CARTESIAN_POINT('Ctrl Pts',(-3.49397567506504,-1.94906001076164,
-0.457587214428717));
#27870=CARTESIAN_POINT('Ctrl Pts',(-3.52013030787576,-1.95285875419799,
0.00168591294888436));
#27871=CARTESIAN_POINT('Ctrl Pts',(-3.62186969212424,-1.95266119647961,
0.00164306867381859));
#27872=CARTESIAN_POINT('Ctrl Pts',(-3.59613206755216,-1.94904494208819,
-0.450423120568937));
#27873=CARTESIAN_POINT('Ctrl Pts',(-3.57039444298008,-1.79274977675162,
-0.904745632987596));
#27874=CARTESIAN_POINT('Ctrl Pts',(-3.54465681840801,-1.50565349219501,
-1.250438408122));
#27875=CARTESIAN_POINT('Ctrl Pts',(-3.50764965271506,-1.09284850536878,
-1.74749709247825));
#27876=CARTESIAN_POINT('Ctrl Pts',(-3.47064248702212,-0.409618924760199,
-2.01996937609925));
#27877=CARTESIAN_POINT('Ctrl Pts',(-3.43363532132918,0.231950860004497,
-1.94339585509611));
#27878=CARTESIAN_POINT('Ctrl Pts',(-3.39662815563624,0.873520644769173,
-1.86682233409297));
#27879=CARTESIAN_POINT('Ctrl Pts',(-3.3596209899433,1.47343063368994,-1.44120300846573));
#27880=CARTESIAN_POINT('Ctrl Pts',(-3.32261382425036,1.75765501167821,-0.860951514885858));
#27881=CARTESIAN_POINT('Ctrl Pts',(-3.28560665855741,2.04187938966649,-0.280700021305966));
#27882=CARTESIAN_POINT('Ctrl Pts',(-3.24859949286447,2.0104181567222,0.454183640226572));
#27883=CARTESIAN_POINT('Ctrl Pts',(-3.21159232717153,1.67764211872612,1.00802062109485));
#27884=CARTESIAN_POINT('Ctrl Pts',(-3.17458516147858,1.34486608073004,1.56185760196311));
#27885=CARTESIAN_POINT('Ctrl Pts',(-3.13757799578564,0.710775237682206,
1.93464790216714));
#27886=CARTESIAN_POINT('Ctrl Pts',(-3.1005708300927,0.0650084742934215,
1.95610903308469));
#27887=CARTESIAN_POINT('Ctrl Pts',(-3.06356366439976,-0.580758289095362,
1.97757016400225));
#27888=CARTESIAN_POINT('Ctrl Pts',(-3.02655649870682,-1.23820097282508,
1.64770212563333));
#27889=CARTESIAN_POINT('Ctrl Pts',(-2.98954933301388,-1.6070140800778,1.11718145235604));
#27890=CARTESIAN_POINT('Ctrl Pts',(-2.96698945271733,-1.83184566054671,
0.79377157592061));
#27891=CARTESIAN_POINT('Ctrl Pts',(-2.94442957242078,-1.94941601300893,
0.395794677332603));
#27892=CARTESIAN_POINT('Ctrl Pts',(-2.92186969212423,-1.95142771007674,
-0.00108710473741568));
#27893=CARTESIAN_POINT('Origin',(-7.7,0.,0.));
#27894=CARTESIAN_POINT('',(-2.12013030787576,-1.95644854722993,-0.00106994229120638));
#27895=CARTESIAN_POINT('',(-2.22186969212423,-1.9565983335214,-0.000961690378010772));
#27896=CARTESIAN_POINT('',(-7.7,-1.954,-2.39295984553393E-16));
#27897=CARTESIAN_POINT('Ctrl Pts',(-2.12013030787576,-1.95644854722993,
-0.00106994229120638));
#27898=CARTESIAN_POINT('Ctrl Pts',(-2.15356351910935,-1.95259121241954,
0.583241937911522));
#27899=CARTESIAN_POINT('Ctrl Pts',(-2.18699673034293,-1.67351864357878,
1.17075110719598));
#27900=CARTESIAN_POINT('Ctrl Pts',(-2.22042994157651,-1.21616753078681,
1.53346843737484));
#27901=CARTESIAN_POINT('Ctrl Pts',(-2.25743710726946,-0.709926347650253,
1.93495964454155));
#27902=CARTESIAN_POINT('Ctrl Pts',(-2.2944442729624,0.0147459708435234,
2.06103051482065));
#27903=CARTESIAN_POINT('Ctrl Pts',(-2.33145143865534,0.626834902648891,
1.85409463186776));
#27904=CARTESIAN_POINT('Ctrl Pts',(-2.36845860434828,1.23892383445426,1.64715874891487));
#27905=CARTESIAN_POINT('Ctrl Pts',(-2.40546577004122,1.73842937957122,1.10721611272997));
#27906=CARTESIAN_POINT('Ctrl Pts',(-2.44247293573417,1.89718828178632,0.480900752167918));
#27907=CARTESIAN_POINT('Ctrl Pts',(-2.47948010142711,2.05594718400142,-0.145414608394115));
#27908=CARTESIAN_POINT('Ctrl Pts',(-2.51648726712005,1.87395944331467,-0.858102693333298));
#27909=CARTESIAN_POINT('Ctrl Pts',(-2.55349443281299,1.4343530975005,-1.33162310690643));
#27910=CARTESIAN_POINT('Ctrl Pts',(-2.59050159850593,0.994746751686315,
-1.80514352047958));
#27911=CARTESIAN_POINT('Ctrl Pts',(-2.62750876419887,0.297521800744686,
-2.03949626268667));
#27912=CARTESIAN_POINT('Ctrl Pts',(-2.66451592989182,-0.338844586481023,
-1.92763410739117));
#27913=CARTESIAN_POINT('Ctrl Pts',(-2.70152309558476,-0.975210973706731,
-1.81577195209567));
#27914=CARTESIAN_POINT('Ctrl Pts',(-2.7385302612777,-1.55071879721652,-1.35769489929758));
#27915=CARTESIAN_POINT('Ctrl Pts',(-2.77553742697064,-1.80248861895329,
-0.762642567579129));
#27916=CARTESIAN_POINT('Ctrl Pts',(-2.79040172060568,-1.90361445468435,
-0.523633920976263));
#27917=CARTESIAN_POINT('Ctrl Pts',(-2.80526601424072,-1.9525114258577,-0.262526962617265));
#27918=CARTESIAN_POINT('Ctrl Pts',(-2.82013030787576,-1.95130973680355,
-0.000989162390181431));
#27919=CARTESIAN_POINT('Ctrl Pts',(-2.92186969212423,-1.95142771007674,
-0.00108710473741568));
#27920=CARTESIAN_POINT('Ctrl Pts',(-2.90742240672784,-1.95271599535519,
-0.255249108206585));
#27921=CARTESIAN_POINT('Ctrl Pts',(-2.89297512133144,-1.90661267726525,
-0.508961994926469));
#27922=CARTESIAN_POINT('Ctrl Pts',(-2.87852783593505,-1.81093858213178,
-0.742354432122333));
#27923=CARTESIAN_POINT('Ctrl Pts',(-2.84152067024211,-1.56586644615734,
-1.34019633513771));
#27924=CARTESIAN_POINT('Ctrl Pts',(-2.80451350454917,-0.995538643432775,
-1.8047068329828));
#27925=CARTESIAN_POINT('Ctrl Pts',(-2.76750633885622,-0.360468490887422,
-1.92370764878637));
#27926=CARTESIAN_POINT('Ctrl Pts',(-2.73049917316328,0.274601661657948,
-2.04270846458994));
#27927=CARTESIAN_POINT('Ctrl Pts',(-2.69349200747034,0.974414164024119,
-1.81619959835197));
#27928=CARTESIAN_POINT('Ctrl Pts',(-2.6564848417774,1.41930990934805,-1.34764536592142));
#27929=CARTESIAN_POINT('Ctrl Pts',(-2.61947767608446,1.86420565467196,-0.879091133490892));
#27930=CARTESIAN_POINT('Ctrl Pts',(-2.58247051039151,2.05418464295365,-0.168491534867828));
#27931=CARTESIAN_POINT('Ctrl Pts',(-2.54546334469857,1.90246861029148,0.459567011909319));
#27932=CARTESIAN_POINT('Ctrl Pts',(-2.50845617900563,1.75075257762931,1.08762555868646));
#27933=CARTESIAN_POINT('Ctrl Pts',(-2.47144901331269,1.25734152402327,1.63314305361767));
#27934=CARTESIAN_POINT('Ctrl Pts',(-2.43444184761975,0.647614871484223,
1.84693898876838));
#27935=CARTESIAN_POINT('Ctrl Pts',(-2.39743468192681,0.0378882189451539,
2.06073492391911));
#27936=CARTESIAN_POINT('Ctrl Pts',(-2.36042751623386,-0.68815403252694,
1.94280929928931));
#27937=CARTESIAN_POINT('Ctrl Pts',(-2.32342035054092,-1.19887159918293,
1.54702797003394));
#27938=CARTESIAN_POINT('Ctrl Pts',(-2.28957013106869,-1.6660217144625,1.1850093012857));
#27939=CARTESIAN_POINT('Ctrl Pts',(-2.25571991159646,-1.95301731563171,
0.590518635644192));
#27940=CARTESIAN_POINT('Ctrl Pts',(-2.22186969212423,-1.9565983335214,-0.000961690378010772));
#27941=CARTESIAN_POINT('Origin',(-7.7,0.,0.));
#27942=CARTESIAN_POINT('',(-1.42013030787576,-1.95447741886037,0.00173992555780794));
#27943=CARTESIAN_POINT('',(-1.52186969212423,-1.95425590186397,0.00176118791910092));
#27944=CARTESIAN_POINT('',(-7.7,-1.954,-2.39295984553393E-16));
#27945=CARTESIAN_POINT('Ctrl Pts',(-1.42013030787576,-1.95447741886037,
0.00173992555780794));
#27946=CARTESIAN_POINT('Ctrl Pts',(-1.42784669259209,-1.95572105433507,
0.136952826586595));
#27947=CARTESIAN_POINT('Ctrl Pts',(-1.43556307730841,-1.94288272355423,
0.271931167846212));
#27948=CARTESIAN_POINT('Ctrl Pts',(-1.44327946202474,-1.915090057649,0.403756738132894));
#27949=CARTESIAN_POINT('Ctrl Pts',(-1.48028662771768,-1.78179864852216,
1.03598165971375));
#27950=CARTESIAN_POINT('Ctrl Pts',(-1.51729379341062,-1.30454480519379,
1.59569016586662));
#27951=CARTESIAN_POINT('Ctrl Pts',(-1.55430095910356,-0.701328365224583,
1.82721860873338));
#27952=CARTESIAN_POINT('Ctrl Pts',(-1.5913081247965,-0.098111925255361,
2.05874705160015));
#27953=CARTESIAN_POINT('Ctrl Pts',(-1.62831529048945,0.631067111354711,
1.96209543118079));
#27954=CARTESIAN_POINT('Ctrl Pts',(-1.66532245618239,1.15313600062339,1.58141262481102));
#27955=CARTESIAN_POINT('Ctrl Pts',(-1.70232962187533,1.67520488989206,1.20072981844126));
#27956=CARTESIAN_POINT('Ctrl Pts',(-1.73933678756827,1.99016363181935,0.536015826121098));
#27957=CARTESIAN_POINT('Ctrl Pts',(-1.77634395326121,1.95414574666676,-0.109102754469346));
#27958=CARTESIAN_POINT('Ctrl Pts',(-1.81335111895415,1.91812786151417,-0.754221335059817));
#27959=CARTESIAN_POINT('Ctrl Pts',(-1.8503582846471,1.53113334928168,-1.37974450392055));
#27960=CARTESIAN_POINT('Ctrl Pts',(-1.88736545034004,0.969932971601319,
-1.69994675904003));
#27961=CARTESIAN_POINT('Ctrl Pts',(-1.92437261603298,0.408732593920964,
-2.02014901415952));
#27962=CARTESIAN_POINT('Ctrl Pts',(-1.96137978172592,-0.326673649207257,
-2.03503035553774));
#27963=CARTESIAN_POINT('Ctrl Pts',(-1.99838694741886,-0.90036825696246,
-1.73779338639092));
#27964=CARTESIAN_POINT('Ctrl Pts',(-2.03539411311181,-1.47406286471766,
-1.4405564172441));
#27965=CARTESIAN_POINT('Ctrl Pts',(-2.07240127880475,-1.88604583709986,
-0.831201137572241));
#27966=CARTESIAN_POINT('Ctrl Pts',(-2.10940844449769,-1.94813229940127,
-0.188067725709169));
#27967=CARTESIAN_POINT('Ctrl Pts',(-2.11298239895705,-1.9541282784138,-0.125957334863212));
#27968=CARTESIAN_POINT('Ctrl Pts',(-2.11655635341641,-1.95686088988079,
-0.0635319066928876));
#27969=CARTESIAN_POINT('Ctrl Pts',(-2.12013030787576,-1.95644854722993,
-0.00106994229120638));
#27970=CARTESIAN_POINT('Ctrl Pts',(-2.22186969212423,-1.9565983335214,-0.000961690378010772));
#27971=CARTESIAN_POINT('Ctrl Pts',(-2.21871274590352,-1.95693230715789,
-0.056124451771436));
#27972=CARTESIAN_POINT('Ctrl Pts',(-2.21555579968281,-1.95480118623589,
-0.111261029713999));
#27973=CARTESIAN_POINT('Ctrl Pts',(-2.2123988534621,-1.95012120828141,-0.166180405709922));
#27974=CARTESIAN_POINT('Ctrl Pts',(-2.17539168776915,-1.89526036888401,
-0.809970418317528));
#27975=CARTESIAN_POINT('Ctrl Pts',(-2.13838452207621,-1.4901458082493,-1.42391340965182));
#27976=CARTESIAN_POINT('Ctrl Pts',(-2.10137735638327,-0.919825037899834,
-1.72757359987075));
#27977=CARTESIAN_POINT('Ctrl Pts',(-2.06437019069033,-0.349504267550385,
-2.03123379008967));
#27978=CARTESIAN_POINT('Ctrl Pts',(-2.02736302499739,0.386022712513811,
-2.02461117919323));
#27979=CARTESIAN_POINT('Ctrl Pts',(-1.99035585930445,0.950783209002053,
-1.7107308219266));
#27980=CARTESIAN_POINT('Ctrl Pts',(-1.9533486936115,1.51554370549031,-1.39685046465995));
#27981=CARTESIAN_POINT('Ctrl Pts',(-1.91634152791856,1.9095377184026,-0.775712361023085));
#27982=CARTESIAN_POINT('Ctrl Pts',(-1.87933436222562,1.95279734749102,-0.131038884865799));
#27983=CARTESIAN_POINT('Ctrl Pts',(-1.84232719653268,1.99605697657943,0.513634591291487));
#27984=CARTESIAN_POINT('Ctrl Pts',(-1.80532003083973,1.68858222184396,1.18184343996919));
#27985=CARTESIAN_POINT('Ctrl Pts',(-1.76831286514679,1.17082088687201,1.56836444964375));
#27986=CARTESIAN_POINT('Ctrl Pts',(-1.73130569945385,0.653059551900069,
1.9548854593183));
#27987=CARTESIAN_POINT('Ctrl Pts',(-1.69429853376091,-0.0749883633083459,
2.05971862998971));
#27988=CARTESIAN_POINT('Ctrl Pts',(-1.65729136806797,-0.680766493625946,
1.83497838636739));
#27989=CARTESIAN_POINT('Ctrl Pts',(-1.62028420237503,-1.28654462394356,
1.61023814274506));
#27990=CARTESIAN_POINT('Ctrl Pts',(-1.58327703668208,-1.77005296937036,
1.05592448482897));
#27991=CARTESIAN_POINT('Ctrl Pts',(-1.54626987098914,-1.91043532921589,
0.425235943498823));
#27992=CARTESIAN_POINT('Ctrl Pts',(-1.53813647803417,-1.94128840524023,
0.286623930317463));
#27993=CARTESIAN_POINT('Ctrl Pts',(-1.5300030850792,-1.95556755240123,0.144322800199925));
#27994=CARTESIAN_POINT('Ctrl Pts',(-1.52186969212423,-1.95425590186397,
0.00176118791910092));
#27995=CARTESIAN_POINT('Origin',(-7.7,0.,0.));
#27996=CARTESIAN_POINT('',(-0.720130307875768,-1.95080492165711,-0.000124213833098269));
#27997=CARTESIAN_POINT('',(-0.821869692124232,-1.95083908144908,-0.000261106490282405));
#27998=CARTESIAN_POINT('',(-7.7,-1.954,-2.39295984553393E-16));
#27999=CARTESIAN_POINT('Ctrl Pts',(-0.720130307875768,-1.95080492165711,
-0.000124213833098269));
#28000=CARTESIAN_POINT('Ctrl Pts',(-0.739137031767772,-1.95059134672475,
0.334498713882938));
#28001=CARTESIAN_POINT('Ctrl Pts',(-0.758143755659777,-1.86892145239226,
0.669217915359824));
#28002=CARTESIAN_POINT('Ctrl Pts',(-0.777150479551781,-1.70640146077838,
0.958534628557673));
#28003=CARTESIAN_POINT('Ctrl Pts',(-0.814157645244724,-1.38996585134649,
1.52185062156551));
#28004=CARTESIAN_POINT('Ctrl Pts',(-0.851164810937665,-0.767025170772472,
1.91304446051378));
#28005=CARTESIAN_POINT('Ctrl Pts',(-0.888171976630607,-0.122157367797084,
1.95338006990175));
#28006=CARTESIAN_POINT('Ctrl Pts',(-0.925179142323548,0.522710435178286,
1.99371567928973));
#28007=CARTESIAN_POINT('Ctrl Pts',(-0.96218630801649,1.18950536055502,1.68319305911744));
#28008=CARTESIAN_POINT('Ctrl Pts',(-0.999193473709431,1.57366693816335,
1.16367700557623));
#28009=CARTESIAN_POINT('Ctrl Pts',(-1.03620063940237,1.95782851577169,0.644160952035009));
#28010=CARTESIAN_POINT('Ctrl Pts',(-1.07320780509532,2.0593567456116,-0.084348534875133));
#28011=CARTESIAN_POINT('Ctrl Pts',(-1.11021497078826,1.83186684979789,-0.689097235990698));
#28012=CARTESIAN_POINT('Ctrl Pts',(-1.1472221364812,1.60437695398418,-1.29384593710626));
#28013=CARTESIAN_POINT('Ctrl Pts',(-1.18422930217414,1.04786893251684,-1.77483385242725));
#28014=CARTESIAN_POINT('Ctrl Pts',(-1.22123646786708,0.416548200503856,
-1.91234932504066));
#28015=CARTESIAN_POINT('Ctrl Pts',(-1.25824363356003,-0.214772531509113,
-2.04986479765406));
#28016=CARTESIAN_POINT('Ctrl Pts',(-1.29525079925297,-0.92090597406773,
-1.8439078275599));
#28017=CARTESIAN_POINT('Ctrl Pts',(-1.33225796494591,-1.37930820788441,
-1.38855867400841));
#28018=CARTESIAN_POINT('Ctrl Pts',(-1.36154874592253,-1.7421287367875,-1.0281546259051));
#28019=CARTESIAN_POINT('Ctrl Pts',(-1.39083952689915,-1.94975667778234,
-0.511517463082888));
#28020=CARTESIAN_POINT('Ctrl Pts',(-1.42013030787576,-1.95447741886037,
0.00173992555780794));
#28021=CARTESIAN_POINT('Ctrl Pts',(-1.52186969212423,-1.95425590186397,
0.00176118791910092));
#28022=CARTESIAN_POINT('Ctrl Pts',(-1.49299591938626,-1.94959950572841,
-0.50433652762779));
#28023=CARTESIAN_POINT('Ctrl Pts',(-1.46412214664829,-1.74845698196316,
-1.01371702142446));
#28024=CARTESIAN_POINT('Ctrl Pts',(-1.43524837391032,-1.39481355369076,
-1.37298340112569));
#28025=CARTESIAN_POINT('Ctrl Pts',(-1.39824120821737,-0.941553044055813,
-1.83345077967584));
#28026=CARTESIAN_POINT('Ctrl Pts',(-1.36123404252443,-0.237775650521653,
-2.04732211203193));
#28027=CARTESIAN_POINT('Ctrl Pts',(-1.32422687683149,0.39504888125557,-1.91690517402407));
#28028=CARTESIAN_POINT('Ctrl Pts',(-1.28721971113855,1.02787341303278,-1.78648823601621));
#28029=CARTESIAN_POINT('Ctrl Pts',(-1.25021254544561,1.58974508305305,-1.31178302764444));
#28030=CARTESIAN_POINT('Ctrl Pts',(-1.21320537975267,1.82401231951764,-0.70962541972142));
#28031=CARTESIAN_POINT('Ctrl Pts',(-1.17619821405972,2.05827955598223,-0.107467811798385));
#28032=CARTESIAN_POINT('Ctrl Pts',(-1.13919104836678,1.96494235889112,0.622142195675899));
#28033=CARTESIAN_POINT('Ctrl Pts',(-1.10218388267384,1.58663671031651,1.14593630401315));
#28034=CARTESIAN_POINT('Ctrl Pts',(-1.0651767169809,1.20833106174192,1.66973041235039));
#28035=CARTESIAN_POINT('Ctrl Pts',(-1.02816955128796,0.545056961683846,
1.9877086215506));
#28036=CARTESIAN_POINT('Ctrl Pts',(-0.991162385595016,-0.100219442561468,
1.95462225401688));
#28037=CARTESIAN_POINT('Ctrl Pts',(-0.954155219902073,-0.745495846806819,
1.92153588648315));
#28038=CARTESIAN_POINT('Ctrl Pts',(-0.91714805420913,-1.37277455523941,
1.53738494221546));
#28039=CARTESIAN_POINT('Ctrl Pts',(-0.880140888516187,-1.69552258335969,
0.977647214365655));
#28040=CARTESIAN_POINT('Ctrl Pts',(-0.860717156385535,-1.86492143156978,
0.683860984439727));
#28041=CARTESIAN_POINT('Ctrl Pts',(-0.841293424254884,-1.9504274654474,
0.341703702312491));
#28042=CARTESIAN_POINT('Ctrl Pts',(-0.821869692124232,-1.95083908144908,
-0.000261106490282405));
#28043=CARTESIAN_POINT('Origin',(-7.7,0.,0.));
#28044=CARTESIAN_POINT('',(-0.0201303078757663,-1.95230810266922,-4.45419903166711E-5));
#28045=CARTESIAN_POINT('',(-0.121869692124238,-1.95503470185946,-0.00140694303418273));
#28046=CARTESIAN_POINT('',(-7.7,-1.954,-2.39295984553393E-16));
#28047=CARTESIAN_POINT('Ctrl Pts',(-0.0201303078757663,-1.95230810266922,
-4.45419903166711E-5));
#28048=CARTESIAN_POINT('Ctrl Pts',(-0.0504273709434536,-1.94838732011207,
0.531290941650261));
#28049=CARTESIAN_POINT('Ctrl Pts',(-0.0807244340111409,-1.72620411445923,
1.06315610289758));
#28050=CARTESIAN_POINT('Ctrl Pts',(-0.111021497078828,-1.34149476870851,
1.42492350079784));
#28051=CARTESIAN_POINT('Ctrl Pts',(-0.148028662771771,-0.871581151338641,
1.86681405654212));
#28052=CARTESIAN_POINT('Ctrl Pts',(-0.185035828464712,-0.159177547940315,
2.0549177184817));
#28053=CARTESIAN_POINT('Ctrl Pts',(-0.222042994157654,0.468425641487877,
1.90068671820305));
#28054=CARTESIAN_POINT('Ctrl Pts',(-0.259050159850595,1.09602883091605,
1.74645571792442));
#28055=CARTESIAN_POINT('Ctrl Pts',(-0.296057325543536,1.63883160637408,
1.24989005542759));
#28056=CARTESIAN_POINT('Ctrl Pts',(-0.333064491236477,1.84974165646342,
0.639034692954403));
#28057=CARTESIAN_POINT('Ctrl Pts',(-0.37007165692942,2.06065170655277,0.0281793304812037));
#28058=CARTESIAN_POINT('Ctrl Pts',(-0.407078822622365,1.9396690312734,-0.696965731968384));
#28059=CARTESIAN_POINT('Ctrl Pts',(-0.444085988315308,1.54162814820921,
-1.20579510892095));
#28060=CARTESIAN_POINT('Ctrl Pts',(-0.48109315400825,1.14358726514503,-1.71462448587351));
#28061=CARTESIAN_POINT('Ctrl Pts',(-0.51810031970119,0.468488174296075,
-2.0071381773291));
#28062=CARTESIAN_POINT('Ctrl Pts',(-0.555107485394131,-0.175075909501228,
-1.9493959880236));
#28063=CARTESIAN_POINT('Ctrl Pts',(-0.592114651087072,-0.818639993298532,
-1.89165379871811));
#28064=CARTESIAN_POINT('Ctrl Pts',(-0.629121816780013,-1.43066907004416,
-1.48365572865153));
#28065=CARTESIAN_POINT('Ctrl Pts',(-0.666128982472954,-1.7317183392721,
-0.911937620084552));
#28066=CARTESIAN_POINT('Ctrl Pts',(-0.684129424273892,-1.87814997618576,
-0.633851515755706));
#28067=CARTESIAN_POINT('Ctrl Pts',(-0.70212986607483,-1.95100718918947,
-0.317031039535227));
#28068=CARTESIAN_POINT('Ctrl Pts',(-0.720130307875768,-1.95080492165711,
-0.000124213833098269));
#28069=CARTESIAN_POINT('Ctrl Pts',(-0.821869692124232,-1.95083908144908,
-0.000261106490282405));
#28070=CARTESIAN_POINT('Ctrl Pts',(-0.804286258561941,-1.95121169895482,
-0.309826511108712));
#28071=CARTESIAN_POINT('Ctrl Pts',(-0.78670282499965,-1.88185055673912,
-0.619234186361387));
#28072=CARTESIAN_POINT('Ctrl Pts',(-0.769119391437359,-1.7418642515495,
-0.892457536920604));
#28073=CARTESIAN_POINT('Ctrl Pts',(-0.732112225744419,-1.44724054381106,
-1.46750004892517));
#28074=CARTESIAN_POINT('Ctrl Pts',(-0.69510506005148,-0.839775780526202,
-1.8822605615025));
#28075=CARTESIAN_POINT('Ctrl Pts',(-0.65809789435854,-0.196925867416372,
-1.94726374474532));
#28076=CARTESIAN_POINT('Ctrl Pts',(-0.621090728665598,0.445924045693496,
-2.01226692798816));
#28077=CARTESIAN_POINT('Ctrl Pts',(-0.584083562972655,1.12415910862834,
-1.72751278189645));
#28078=CARTESIAN_POINT('Ctrl Pts',(-0.547076397279713,1.52793680192538,
-1.22311221086593));
#28079=CARTESIAN_POINT('Ctrl Pts',(-0.51006923158677,1.93171449522242,-0.718711639835416));
#28080=CARTESIAN_POINT('Ctrl Pts',(-0.473062065893828,2.06103481888165,
0.00533535613392075));
#28081=CARTESIAN_POINT('Ctrl Pts',(-0.436054900200886,1.8569022710431,0.618378693290504));
#28082=CARTESIAN_POINT('Ctrl Pts',(-0.399047734507945,1.65276972320455,
1.23142203044707));
#28083=CARTESIAN_POINT('Ctrl Pts',(-0.362040568815004,1.11518430386824,
1.73346170879089));
#28084=CARTESIAN_POINT('Ctrl Pts',(-0.325033403122063,0.489560150069195,
1.89502691947245));
#28085=CARTESIAN_POINT('Ctrl Pts',(-0.288026237429121,-0.136064003729868,
2.05659213015401));
#28086=CARTESIAN_POINT('Ctrl Pts',(-0.251019071736179,-0.849726891991672,
1.87768287317329));
#28087=CARTESIAN_POINT('Ctrl Pts',(-0.214011906043236,-1.32516987168342,
1.4403068683668));
#28088=CARTESIAN_POINT('Ctrl Pts',(-0.183297834736904,-1.7197634404401,
1.07730695881503));
#28089=CARTESIAN_POINT('Ctrl Pts',(-0.152583763430571,-1.95026736215908,
0.536271058584337));
#28090=CARTESIAN_POINT('Ctrl Pts',(-0.121869692124238,-1.95503470185946,
-0.00140694303418273));
#28091=CARTESIAN_POINT('Origin',(-16.9400562256037,0.,0.));
#28092=CARTESIAN_POINT('',(-0.490056225603702,-1.55295652796194,-9.88815851658073E-5));
#28093=CARTESIAN_POINT('',(-0.351943774396294,-1.55632368410563,-0.00112001017909952));
#28094=CARTESIAN_POINT('',(-16.9400562256037,-1.5555,-7.70311135908521E-14));
#28095=CARTESIAN_POINT('',(0.,0.4799292661563,1.47961081014119));
#28096=CARTESIAN_POINT('Ctrl Pts',(-0.490056225603702,-1.55295652796194,
-9.88815851658657E-5));
#28097=CARTESIAN_POINT('Ctrl Pts',(-0.472055783802765,-1.55311754492539,
-0.252375528145892));
#28098=CARTESIAN_POINT('Ctrl Pts',(-0.417048176308885,-1.37587923427884,
-1.0230984760672));
#28099=CARTESIAN_POINT('Ctrl Pts',(-0.325033403122065,-0.164474555116665,
-1.83065940731556));
#28100=CARTESIAN_POINT('Ctrl Pts',(-0.21401190604324,1.4477823064221,-1.13208461653888));
#28101=CARTESIAN_POINT('Ctrl Pts',(-0.105667438335883,1.72974363970491,
0.557933133189484));
#28102=CARTESIAN_POINT('Ctrl Pts',(-0.0343301363214699,0.933636559814803,
1.33261642798006));
#28103=CARTESIAN_POINT('Ctrl Pts',(1.07607065619186E-15,0.480182858679997,
1.4822056829043));
#28104=CARTESIAN_POINT('',(2.22044604925031E-15,1.55526325306019,0.0271378643346999));
#28105=CARTESIAN_POINT('Origin',(0.,0.,0.));
#28106=CARTESIAN_POINT('Ctrl Pts',(-0.351943774396294,-1.55632368410563,
-0.00112001017909957));
#28107=CARTESIAN_POINT('Ctrl Pts',(-0.345650680009688,-1.55710127006918,
-0.0888189981367454));
#28108=CARTESIAN_POINT('Ctrl Pts',(-0.302350419930139,-1.51054435461524,
-0.691468448221064));
#28109=CARTESIAN_POINT('Ctrl Pts',(-0.222042994157651,-0.72473494787801,
-1.69026698927826));
#28110=CARTESIAN_POINT('Ctrl Pts',(-0.111021497078823,1.0270020972766,-1.52351327282068));
#28111=CARTESIAN_POINT('Ctrl Pts',(-0.03700716569294,1.56427778786756,-0.489482550463674));
#28112=CARTESIAN_POINT('Ctrl Pts',(2.22044604925031E-15,1.55526325306019,
0.0271378643346999));
#28113=CARTESIAN_POINT('Origin',(-16.9400562256037,0.,0.));
#28114=CARTESIAN_POINT('',(-1.1900562256037,-1.55588005375502,0.00138508403538328));
#28115=CARTESIAN_POINT('',(-1.05194377439629,-1.55298372118426,-0.000207856267061268));
#28116=CARTESIAN_POINT('',(-16.9400562256037,-1.5555,-7.70311135908521E-14));
#28117=CARTESIAN_POINT('Ctrl Pts',(-1.1900562256037,-1.55588005375502,0.00138508403538323));
#28118=CARTESIAN_POINT('Ctrl Pts',(-1.16076544462708,-1.5521220636082,-0.407198267054996));
#28119=CARTESIAN_POINT('Ctrl Pts',(-1.09446749795752,-1.17801114814899,
-1.33809225472144));
#28120=CARTESIAN_POINT('Ctrl Pts',(-0.991162385595018,0.391152455034581,
-1.79576804489885));
#28121=CARTESIAN_POINT('Ctrl Pts',(-0.880140888516193,1.72019272226962,
-0.647083240986163));
#28122=CARTESIAN_POINT('Ctrl Pts',(-0.769119391437366,1.47772522761866,
1.09272715853592));
#28123=CARTESIAN_POINT('Ctrl Pts',(-0.658097894358541,-0.114699807832016,
1.83431047841002));
#28124=CARTESIAN_POINT('Ctrl Pts',(-0.565076839080654,-1.36118632868951,
1.05154277275593));
#28125=CARTESIAN_POINT('Ctrl Pts',(-0.509062949495707,-1.55278650963683,
0.266280833902191));
#28126=CARTESIAN_POINT('Ctrl Pts',(-0.490056225603702,-1.55295652796194,
-9.88815851658657E-5));
#28127=CARTESIAN_POINT('Ctrl Pts',(-1.05194377439629,-1.55298372118426,
-0.000207856267061286));
#28128=CARTESIAN_POINT('Ctrl Pts',(-1.034360340834,-1.5532803468394,-0.24664029581869));
#28129=CARTESIAN_POINT('Ctrl Pts',(-0.979769741578774,-1.38185467141502,
-1.01133963636197));
#28130=CARTESIAN_POINT('Ctrl Pts',(-0.888171976630605,-0.184933360961542,
-1.82856513855231));
#28131=CARTESIAN_POINT('Ctrl Pts',(-0.777150479551777,1.43481276042301,
-1.14852152405029));
#28132=CARTESIAN_POINT('Ctrl Pts',(-0.666128982472953,1.74365272478113,
0.580631652352415));
#28133=CARTESIAN_POINT('Ctrl Pts',(-0.555107485394127,0.459803001478689,
1.7795918156029));
#28134=CARTESIAN_POINT('Ctrl Pts',(-0.450379082701908,-1.14794220903712,
1.37654367374382));
#28135=CARTESIAN_POINT('Ctrl Pts',(-0.38265784570263,-1.55252859868912,
0.426903598581234));
#28136=CARTESIAN_POINT('Ctrl Pts',(-0.351943774396294,-1.55632368410563,
-0.00112001017909957));
#28137=CARTESIAN_POINT('Origin',(-16.9400562256037,0.,0.));
#28138=CARTESIAN_POINT('',(-1.8900562256037,-1.55744918895402,-0.000851737581328525));
#28139=CARTESIAN_POINT('',(-1.75194377439629,-1.55570371307544,0.00140201013713322));
#28140=CARTESIAN_POINT('',(-16.9400562256037,-1.5555,-7.70311135908521E-14));
#28141=CARTESIAN_POINT('Ctrl Pts',(-1.8900562256037,-1.55744918895402,-0.000851737581328577));
#28142=CARTESIAN_POINT('Ctrl Pts',(-1.88648227114434,-1.557777438183,-0.0505751693248516));
#28143=CARTESIAN_POINT('Ctrl Pts',(-1.84590115099204,-1.53307735824119,
-0.614838726303634));
#28144=CARTESIAN_POINT('Ctrl Pts',(-1.7683128651468,-0.845478645101226,
-1.63185140458178));
#28145=CARTESIAN_POINT('Ctrl Pts',(-1.65729136806797,0.910802436555798,
-1.59631211106002));
#28146=CARTESIAN_POINT('Ctrl Pts',(-1.54626987098914,1.83501425402401,-0.102451380513119));
#28147=CARTESIAN_POINT('Ctrl Pts',(-1.43524837391032,1.08283668534245,1.48500401619214));
#28148=CARTESIAN_POINT('Ctrl Pts',(-1.32422687683149,-0.658572718107321,
1.71582529904111));
#28149=CARTESIAN_POINT('Ctrl Pts',(-1.24249616072929,-1.49763533076483,
0.731798689168104));
#28150=CARTESIAN_POINT('Ctrl Pts',(-1.19777261032002,-1.5568700614218,0.109022580222819));
#28151=CARTESIAN_POINT('Ctrl Pts',(-1.1900562256037,-1.55588005375502,0.00138508403538323));
#28152=CARTESIAN_POINT('Ctrl Pts',(-1.75194377439629,-1.55570371307544,
0.00140201013713313));
#28153=CARTESIAN_POINT('Ctrl Pts',(-1.72307000165832,-1.55199694532266,
-0.401481816133661));
#28154=CARTESIAN_POINT('Ctrl Pts',(-1.65718906322741,-1.1866499045939,-1.32669967921838));
#28155=CARTESIAN_POINT('Ctrl Pts',(-1.55430095910356,0.370965051819814,
-1.80004421839588));
#28156=CARTESIAN_POINT('Ctrl Pts',(-1.44327946202473,1.71281466704483,-0.6663636376042));
#28157=CARTESIAN_POINT('Ctrl Pts',(-1.33225796494591,1.48990881738992,1.0760750010236));
#28158=CARTESIAN_POINT('Ctrl Pts',(-1.22123646786708,-0.0941078601541336,
1.83546359530854));
#28159=CARTESIAN_POINT('Ctrl Pts',(-1.12779840435054,-1.35490149413674,
1.06334259309671));
#28160=CARTESIAN_POINT('Ctrl Pts',(-1.07136750652695,-1.55265605041119,
0.272016432419122));
#28161=CARTESIAN_POINT('Ctrl Pts',(-1.05194377439629,-1.55298372118426,
-0.000207856267061286));
#28162=CARTESIAN_POINT('Origin',(-16.9400562256037,0.,0.));
#28163=CARTESIAN_POINT('',(-2.5900562256037,-1.55335839078706,-0.000787431984669446));
#28164=CARTESIAN_POINT('',(-2.45194377439629,-1.55756842773415,-0.000765562632226713));
#28165=CARTESIAN_POINT('',(-16.9400562256037,-1.5555,-7.70311135908521E-14));
#28166=CARTESIAN_POINT('Ctrl Pts',(-2.5900562256037,-1.55335839078706,-0.000787431984669417));
#28167=CARTESIAN_POINT('Ctrl Pts',(-2.57519193196866,-1.55431500661292,
-0.208987047262663));
#28168=CARTESIAN_POINT('Ctrl Pts',(-2.52332047264068,-1.41848003230292,
-0.934337843636373));
#28169=CARTESIAN_POINT('Ctrl Pts',(-2.43444184761975,-0.31818743609586,
-1.81011879586092));
#28170=CARTESIAN_POINT('Ctrl Pts',(-2.32342035054093,1.34690991987603,-1.25044271013452));
#28171=CARTESIAN_POINT('Ctrl Pts',(-2.2123988534621,1.78152905596337,0.45158336374919));
#28172=CARTESIAN_POINT('Ctrl Pts',(-2.10137735638328,0.588620854178164,
1.74106254069739));
#28173=CARTESIAN_POINT('Ctrl Pts',(-1.99392981376381,-1.08631350257498,
1.44967507269646));
#28174=CARTESIAN_POINT('Ctrl Pts',(-1.92348943683728,-1.5543785214527,0.464295206971033));
#28175=CARTESIAN_POINT('Ctrl Pts',(-1.8900562256037,-1.55744918895402,-0.000851737581328577));
#28176=CARTESIAN_POINT('Ctrl Pts',(-2.45194377439629,-1.55756842773415,
-0.0007655626322266));
#28177=CARTESIAN_POINT('Ctrl Pts',(-2.44878682817558,-1.55783429057528,
-0.0446783954609667));
#28178=CARTESIAN_POINT('Ctrl Pts',(-2.40862271626193,-1.53625065827796,
-0.603092332538515));
#28179=CARTESIAN_POINT('Ctrl Pts',(-2.33145143865534,-0.863749286419899,
-1.62225467335409));
#28180=CARTESIAN_POINT('Ctrl Pts',(-2.22042994157651,0.892820136543068,
-1.60643869907147));
#28181=CARTESIAN_POINT('Ctrl Pts',(-2.10940844449769,1.8337480082192,-0.123050285242695));
#28182=CARTESIAN_POINT('Ctrl Pts',(-1.99838694741886,1.09944353382152,1.47275145086502));
#28183=CARTESIAN_POINT('Ctrl Pts',(-1.88736545034003,-0.639264550272716,
1.72311173281902));
#28184=CARTESIAN_POINT('Ctrl Pts',(-1.80521772599918,-1.49366042548188,
0.74359750648739));
#28185=CARTESIAN_POINT('Ctrl Pts',(-1.76007716735126,-1.55674786476977,
0.114889516740449));
#28186=CARTESIAN_POINT('Ctrl Pts',(-1.75194377439629,-1.55570371307544,
0.00140201013713313));
#28187=CARTESIAN_POINT('Origin',(-16.9400562256037,0.,0.));
#28188=CARTESIAN_POINT('',(-3.29005622560369,-1.55459150059108,0.00134208679213341));
#28189=CARTESIAN_POINT('',(-3.15194377439629,-1.55345230451605,-0.000865399907588604));
#28190=CARTESIAN_POINT('',(-16.9400562256037,-1.5555,-7.70311135908521E-14));
#28191=CARTESIAN_POINT('Ctrl Pts',(-3.29005622560369,-1.55459150059108,
0.00134208679213352));
#28192=CARTESIAN_POINT('Ctrl Pts',(-3.26390159279297,-1.55156747530179,
-0.364266587535299));
#28193=CARTESIAN_POINT('Ctrl Pts',(-3.20073979428931,-1.24038640780706,
-1.25182269198089));
#28194=CARTESIAN_POINT('Ctrl Pts',(-3.1005708300927,0.238288506115619,-1.82235888080426));
#28195=CARTESIAN_POINT('Ctrl Pts',(-2.98954933301389,1.65947641764626,-0.789880574454531));
#28196=CARTESIAN_POINT('Ctrl Pts',(-2.87852783593505,1.5646389708752,0.964198212866461));
#28197=CARTESIAN_POINT('Ctrl Pts',(-2.76750633885623,0.0404155252740006,
1.83742751899441));
#28198=CARTESIAN_POINT('Ctrl Pts',(-2.67134913541244,-1.31171330547879,
1.13989061901984));
#28199=CARTESIAN_POINT('Ctrl Pts',(-2.6121990976616,-1.55193335019243,0.309361005391319));
#28200=CARTESIAN_POINT('Ctrl Pts',(-2.5900562256037,-1.55335839078706,-0.000787431984669417));
#28201=CARTESIAN_POINT('Ctrl Pts',(-3.15194377439629,-1.55345230451605,
-0.000865399907588483));
#28202=CARTESIAN_POINT('Ctrl Pts',(-3.1374964889999,-1.55447785607725,-0.203193443099082));
#28203=CARTESIAN_POINT('Ctrl Pts',(-3.08604203791056,-1.4237661941345,-0.922517657784447));
#28204=CARTESIAN_POINT('Ctrl Pts',(-2.99758042112829,-0.338493072017185,
-1.8064317083433));
#28205=CARTESIAN_POINT('Ctrl Pts',(-2.88655892404946,1.33278381758959,-1.26548819539577));
#28206=CARTESIAN_POINT('Ctrl Pts',(-2.77553742697064,1.78648747614462,0.431550201213581));
#28207=CARTESIAN_POINT('Ctrl Pts',(-2.66451592989181,0.608134005493306,
1.73434313370923));
#28208=CARTESIAN_POINT('Ctrl Pts',(-2.5566513790337,-1.07647945219465,1.46072394163763));
#28209=CARTESIAN_POINT('Ctrl Pts',(-2.48579399386852,-1.55471772490545,
0.470087890350195));
#28210=CARTESIAN_POINT('Ctrl Pts',(-2.45194377439629,-1.55756842773415,
-0.0007655626322266));
#28211=CARTESIAN_POINT('Origin',(-16.9400562256037,0.,0.));
#28212=CARTESIAN_POINT('',(-3.9900562256037,-1.55802831486089,-0.000113059531867663));
#28213=CARTESIAN_POINT('',(-3.85194377439629,-1.55443423291916,0.00130798020558064));
#28214=CARTESIAN_POINT('',(-16.9400562256037,-1.5555,-7.70311135908521E-14));
#28215=CARTESIAN_POINT('Ctrl Pts',(-3.9900562256037,-1.55802831486089,-0.000113059531867614));
#28216=CARTESIAN_POINT('Ctrl Pts',(-3.98961841931024,-1.55803469606833,
-0.00619811891591143));
#28217=CARTESIAN_POINT('Ctrl Pts',(-3.95217344732383,-1.55524873298545,
-0.526638897489874));
#28218=CARTESIAN_POINT('Ctrl Pts',(-3.87772130964449,-0.980111674806025,
-1.55472004153636));
#28219=CARTESIAN_POINT('Ctrl Pts',(-3.76669981256566,0.772908208897534,
-1.66744901069363));
#28220=CARTESIAN_POINT('Ctrl Pts',(-3.65567831548684,1.81983282548855,-0.256869207804794));
#28221=CARTESIAN_POINT('Ctrl Pts',(-3.54465681840801,1.20423745559398,1.38837511256683));
#28222=CARTESIAN_POINT('Ctrl Pts',(-3.43363532132918,-0.511496789897079,
1.76526041607566));
#28223=CARTESIAN_POINT('Ctrl Pts',(-3.34876845706108,-1.46583715960521,
0.820607790786356));
#28224=CARTESIAN_POINT('Ctrl Pts',(-3.30090875848592,-1.5558462814984,0.153046765228203));
#28225=CARTESIAN_POINT('Ctrl Pts',(-3.29005622560369,-1.55459150059108,
0.00134208679213352));
#28226=CARTESIAN_POINT('Ctrl Pts',(-3.85194377439629,-1.55443423291916,
0.00130798020558057));
#28227=CARTESIAN_POINT('Ctrl Pts',(-3.82620614982422,-1.55155547974314,
-0.358563543523688));
#28228=CARTESIAN_POINT('Ctrl Pts',(-3.7634613595592,-1.24823606413057,-1.24025965145944));
#28229=CARTESIAN_POINT('Ctrl Pts',(-3.66370940360124,0.217810325062528,
-1.82491965286328));
#28230=CARTESIAN_POINT('Ctrl Pts',(-3.55268790652242,1.65050222030251,-0.808464902075287));
#28231=CARTESIAN_POINT('Ctrl Pts',(-3.4416664094436,1.57536719290506,0.946568161661344));
#28232=CARTESIAN_POINT('Ctrl Pts',(-3.33064491236476,0.0610453305290268,
1.83685779108923));
#28233=CARTESIAN_POINT('Ctrl Pts',(-3.23407070068233,-1.30472822637037,
1.15158886161436));
#28234=CARTESIAN_POINT('Ctrl Pts',(-3.17450365469284,-1.5518508742249,0.315076059667656));
#28235=CARTESIAN_POINT('Ctrl Pts',(-3.15194377439629,-1.55345230451605,
-0.000865399907588483));
#28236=CARTESIAN_POINT('Origin',(-16.9400562256037,0.,0.));
#28237=CARTESIAN_POINT('',(-4.6900562256037,-1.55426764476375,-0.00126339721357951));
#28238=CARTESIAN_POINT('',(-4.55194377439629,-1.55803858294675,-5.37804637934514E-6));
#28239=CARTESIAN_POINT('',(-16.9400562256037,-1.5555,-7.70311135908521E-14));
#28240=CARTESIAN_POINT('Ctrl Pts',(-4.6900562256037,-1.55426764476375,-0.00126339721357914));
#28241=CARTESIAN_POINT('Ctrl Pts',(-4.67832808013455,-1.55552512007785,
-0.165294437232494));
#28242=CARTESIAN_POINT('Ctrl Pts',(-4.62959276897247,-1.45615629828598,
-0.845427058906527));
#28243=CARTESIAN_POINT('Ctrl Pts',(-4.54385029211744,-0.469736383593091,
-1.77682892608546));
#28244=CARTESIAN_POINT('Ctrl Pts',(-4.43282879503861,1.2366354145067,-1.35959779134602));
#28245=CARTESIAN_POINT('Ctrl Pts',(-4.32180729795979,1.8132709732004,0.299702653298089));
#28246=CARTESIAN_POINT('Ctrl Pts',(-4.21078580088097,0.733381167783709,
1.68520781074188));
#28247=CARTESIAN_POINT('Ctrl Pts',(-4.1002021100956,-1.00959320041139,1.53178792699158));
#28248=CARTESIAN_POINT('Ctrl Pts',(-4.02662558500318,-1.55749530135286,
0.50816360735401));
#28249=CARTESIAN_POINT('Ctrl Pts',(-3.9900562256037,-1.55802831486089,-0.000113059531867614));
#28250=CARTESIAN_POINT('Ctrl Pts',(-4.55194377439629,-1.55803858294675,
-5.37804637950411E-6));
#28251=CARTESIAN_POINT('Ctrl Pts',(-4.55192297634147,-1.55803859780055,
-0.000294444541598174));
#28252=CARTESIAN_POINT('Ctrl Pts',(-4.51489501259372,-1.55790772834933,
-0.514936006620134));
#28253=CARTESIAN_POINT('Ctrl Pts',(-4.44085988315302,-0.997507700137877,
-1.5436163594892));
#28254=CARTESIAN_POINT('Ctrl Pts',(-4.3298383860742,0.754135777011385,-1.67602276444812));
#28255=CARTESIAN_POINT('Ctrl Pts',(-4.21881688899538,1.81683366297973,-0.277287789454163));
#28256=CARTESIAN_POINT('Ctrl Pts',(-4.10779539191654,1.21975146666773,1.37476522965911));
#28257=CARTESIAN_POINT('Ctrl Pts',(-3.99677389483772,-0.491642529871626,
1.77089262800929));
#28258=CARTESIAN_POINT('Ctrl Pts',(-3.91149002233097,-1.46127128776662,
0.832427049795263));
#28259=CARTESIAN_POINT('Ctrl Pts',(-3.86321331551716,-1.55569473103557,
0.158882231999483));
#28260=CARTESIAN_POINT('Ctrl Pts',(-3.85194377439629,-1.55443423291916,
0.00130798020558057));
#28261=CARTESIAN_POINT('Origin',(-16.9400562256037,0.,0.));
#28262=CARTESIAN_POINT('',(-5.3900562256037,-1.55356607152694,0.000946640642580529));
#28263=CARTESIAN_POINT('',(-5.25194377439629,-1.55441883725758,-0.00130423800998869));
#28264=CARTESIAN_POINT('',(-16.9400562256037,-1.5555,-7.70311135908521E-14));
#28265=CARTESIAN_POINT('Ctrl Pts',(-5.3900562256037,-1.55356607152694,0.000946640642580637));
#28266=CARTESIAN_POINT('Ctrl Pts',(-5.36703774095887,-1.55177070227827,
-0.321358232211269));
#28267=CARTESIAN_POINT('Ctrl Pts',(-5.30701209062111,-1.29693323687991,
-1.16443930671404));
#28268=CARTESIAN_POINT('Ctrl Pts',(-5.20997927459039,0.0837239529942017,
-1.83596394363836));
#28269=CARTESIAN_POINT('Ctrl Pts',(-5.09895777751157,1.58693624990787,-0.927041876817589));
#28270=CARTESIAN_POINT('Ctrl Pts',(-4.98793628043274,1.64039272540732,0.828785261135749));
#28271=CARTESIAN_POINT('Ctrl Pts',(-4.87691478335392,0.195257872362318,
1.82747029139345));
#28272=CARTESIAN_POINT('Ctrl Pts',(-4.77762143174423,-1.25675047370399,
1.22752168128547));
#28273=CARTESIAN_POINT('Ctrl Pts',(-4.71533524582749,-1.55155726365705,
0.352291560718858));
#28274=CARTESIAN_POINT('Ctrl Pts',(-4.6900562256037,-1.55426764476375,-0.00126339721357914));
#28275=CARTESIAN_POINT('Ctrl Pts',(-5.25194377439629,-1.55441883725758,
-0.00130423800998841));
#28276=CARTESIAN_POINT('Ctrl Pts',(-5.2406326371658,-1.55567946829412,-0.159464061065563));
#28277=CARTESIAN_POINT('Ctrl Pts',(-5.19231433424236,-1.46081140823039,
-0.833606098981985));
#28278=CARTESIAN_POINT('Ctrl Pts',(-5.10698886562598,-0.489658649608892,
-1.77144220452719));
#28279=CARTESIAN_POINT('Ctrl Pts',(-4.99596736854715,1.22129057217261,-1.37339812706995));
#28280=CARTESIAN_POINT('Ctrl Pts',(-4.88494587146833,1.81652193399072,0.279322645783608));
#28281=CARTESIAN_POINT('Ctrl Pts',(-4.77392437438949,0.752257995551791,
1.67686641842616));
#28282=CARTESIAN_POINT('Ctrl Pts',(-4.66292367536549,-0.998907961074514,
1.54252325729719));
#28283=CARTESIAN_POINT('Ctrl Pts',(-4.58893014203442,-1.55801216758575,
0.514058064897643));
#28284=CARTESIAN_POINT('Ctrl Pts',(-4.55194377439629,-1.55803858294675,
-5.37804637950411E-6));
#28285=CARTESIAN_POINT('Origin',(-16.9400562256037,0.,0.));
#28286=CARTESIAN_POINT('',(-6.0900562256037,-1.55768689774605,0.000665455443045115));
#28287=CARTESIAN_POINT('',(-5.95194377439629,-1.55346217675642,0.000872969649942032));
#28288=CARTESIAN_POINT('',(-16.9400562256037,-1.5555,-7.70311135908521E-14));
#28289=CARTESIAN_POINT('Ctrl Pts',(-6.0900562256037,-1.55768689774605,0.000665455443045072));
#28290=CARTESIAN_POINT('Ctrl Pts',(-6.05574740178319,-1.5551166351628,-0.476471113420595));
#28291=CARTESIAN_POINT('Ctrl Pts',(-5.98443141226975,-1.06553522999869,
-1.47283120294195));
#28292=CARTESIAN_POINT('Ctrl Pts',(-5.87610825706334,0.629504981698008,
-1.72670112661761));
#28293=CARTESIAN_POINT('Ctrl Pts',(-5.76508675998453,1.79168050778642,-0.409456054617966));
#28294=CARTESIAN_POINT('Ctrl Pts',(-5.65406526290569,1.31705477835589,1.28185023050864));
#28295=CARTESIAN_POINT('Ctrl Pts',(-5.54304376582688,-0.360774817741443,
1.80211399015954));
#28296=CARTESIAN_POINT('Ctrl Pts',(-5.45504075339287,-1.42948053097645,
0.909516853134372));
#28297=CARTESIAN_POINT('Ctrl Pts',(-5.40404490665181,-1.55465714455676,
0.196816183584846));
#28298=CARTESIAN_POINT('Ctrl Pts',(-5.3900562256037,-1.55356607152694,0.000946640642580637));
#28299=CARTESIAN_POINT('Ctrl Pts',(-5.95194377439629,-1.55346217675642,
0.000872969649942171));
#28300=CARTESIAN_POINT('Ctrl Pts',(-5.92934229799011,-1.55184313839371,
-0.315645984838267));
#28301=CARTESIAN_POINT('Ctrl Pts',(-5.86973365589099,-1.30402610796483,
-1.15275506404449));
#28302=CARTESIAN_POINT('Ctrl Pts',(-5.77311784809893,0.0631027514921653,
-1.83678826212252));
#28303=CARTESIAN_POINT('Ctrl Pts',(-5.6620963510201,1.57642645299097,-0.944803003502463));
#28304=CARTESIAN_POINT('Ctrl Pts',(-5.55107485394128,1.64959562566877,0.810313117807789));
#28305=CARTESIAN_POINT('Ctrl Pts',(-5.44005335686245,0.215766101057041,
1.82516247680901));
#28306=CARTESIAN_POINT('Ctrl Pts',(-5.34034299701413,-1.24901343126791,
1.23910521287792));
#28307=CARTESIAN_POINT('Ctrl Pts',(-5.27763980285874,-1.5515550039988,0.357994675267643));
#28308=CARTESIAN_POINT('Ctrl Pts',(-5.25194377439629,-1.55441883725758,
-0.00130423800998841));
#28309=CARTESIAN_POINT('Origin',(-16.9400562256037,0.,0.));
#28310=CARTESIAN_POINT('',(-6.7900562256037,-1.55551006981711,-0.00141244968499829));
#28311=CARTESIAN_POINT('',(-6.65194377439629,-1.55757973858287,0.000756704723131347));
#28312=CARTESIAN_POINT('',(-16.9400562256037,-1.5555,-7.70311135908521E-14));
#28313=CARTESIAN_POINT('Ctrl Pts',(-6.7900562256037,-1.55551006981711,-0.00141244968499835));
#28314=CARTESIAN_POINT('Ctrl Pts',(-6.78146422830045,-1.55660813262382,
-0.121337247012077));
#28315=CARTESIAN_POINT('Ctrl Pts',(-6.73586506530426,-1.48920084493374,
-0.756577051035784));
#28316=CARTESIAN_POINT('Ctrl Pts',(-6.65325873661513,-0.617937253968403,
-1.73087459187634));
#28317=CARTESIAN_POINT('Ctrl Pts',(-6.5422372395363,1.11754670885474,-1.45906225232958));
#28318=CARTESIAN_POINT('Ctrl Pts',(-6.43121574245748,1.83208868553414,0.145685795405434));
#28319=CARTESIAN_POINT('Ctrl Pts',(-6.32019424537864,0.872914255927876,
1.6173416474088));
#28320=CARTESIAN_POINT('Ctrl Pts',(-6.20917274829983,-0.883716608491293,
1.61146463148335));
#28321=CARTESIAN_POINT('Ctrl Pts',(-6.13246007504151,-1.53965976377384,
0.590180722825843));
#28322=CARTESIAN_POINT('Ctrl Pts',(-6.09275456747613,-1.55788904536813,
0.0381915912665651));
#28323=CARTESIAN_POINT('Ctrl Pts',(-6.0900562256037,-1.55768689774605,0.000665455443045072));
#28324=CARTESIAN_POINT('Ctrl Pts',(-6.65194377439629,-1.55757973858287,
0.000756704723131364));
#28325=CARTESIAN_POINT('Ctrl Pts',(-6.61805195881443,-1.55475278059858,
-0.470666295640637));
#28326=CARTESIAN_POINT('Ctrl Pts',(-6.54715297753963,-1.07549238527194,
-1.4618239969165));
#28327=CARTESIAN_POINT('Ctrl Pts',(-6.43924683057189,0.610076257496618,
-1.73366087720635));
#28328=CARTESIAN_POINT('Ctrl Pts',(-6.32822533349305,1.78696973330201,-0.429548890557871));
#28329=CARTESIAN_POINT('Ctrl Pts',(-6.21720383641424,1.3313655119277,1.26698024876731));
#28330=CARTESIAN_POINT('Ctrl Pts',(-6.10618233933541,-0.340516238842866,
1.80605143010969));
#28331=CARTESIAN_POINT('Ctrl Pts',(-6.01776231866276,-1.42428876297189,
0.92133852484065));
#28332=CARTESIAN_POINT('Ctrl Pts',(-5.96634946368305,-1.55449411658094,
0.202615264258711));
#28333=CARTESIAN_POINT('Ctrl Pts',(-5.95194377439629,-1.55346217675642,
0.000872969649942171));
#28334=CARTESIAN_POINT('Origin',(-16.9400562256037,0.,0.));
#28335=CARTESIAN_POINT('',(-7.4900562256037,-1.5530180908049,0.000313254609165155));
#28336=CARTESIAN_POINT('',(-7.3519437743963,-1.55568612057705,-0.00140331110564815));
#28337=CARTESIAN_POINT('',(-16.9400562256037,-1.5555,-7.70311135908521E-14));
#28338=CARTESIAN_POINT('Ctrl Pts',(-7.4900562256037,-1.5530180908049,0.000313254609165155));
#28339=CARTESIAN_POINT('Ctrl Pts',(-7.47017388912477,-1.55251547593583,
-0.278325135901937));
#28340=CARTESIAN_POINT('Ctrl Pts',(-7.4132843869529,-1.34789754076425,-1.07628426120452));
#28341=CARTESIAN_POINT('Ctrl Pts',(-7.31938771908807,-0.0714373480345857,
-1.8364830540876));
#28342=CARTESIAN_POINT('Ctrl Pts',(-7.20836622200926,1.50308509085693,-1.05759562796407));
#28343=CARTESIAN_POINT('Ctrl Pts',(-7.09734472493043,1.70445447418163,0.687465088631667));
#28344=CARTESIAN_POINT('Ctrl Pts',(-6.9863232278516,0.348708506197304,1.80448765037358));
#28345=CARTESIAN_POINT('Ctrl Pts',(-6.88389372807603,-1.19602678497936,
1.31414025780625));
#28346=CARTESIAN_POINT('Ctrl Pts',(-6.81847139399339,-1.55187859293768,
0.39519886080267));
#28347=CARTESIAN_POINT('Ctrl Pts',(-6.7900562256037,-1.55551006981711,-0.00141244968499835));
#28348=CARTESIAN_POINT('Ctrl Pts',(-7.3519437743963,-1.55568612057705,-0.00140331110564832));
#28349=CARTESIAN_POINT('Ctrl Pts',(-7.3437687853317,-1.55673540772934,-0.115474538019075));
#28350=CARTESIAN_POINT('Ctrl Pts',(-7.29858663057415,-1.49325970695437,
-0.744774653469687));
#28351=CARTESIAN_POINT('Ctrl Pts',(-7.21639731012365,-0.637334153250706,
-1.723826631137));
#28352=CARTESIAN_POINT('Ctrl Pts',(-7.10537581304485,1.10109249863036,-1.47151907448626));
#28353=CARTESIAN_POINT('Ctrl Pts',(-6.994354315966,1.83360901398418,0.125104200380868));
#28354=CARTESIAN_POINT('Ctrl Pts',(-6.8833328188872,0.891020217215038,1.60743772807255));
#28355=CARTESIAN_POINT('Ctrl Pts',(-6.77231132180836,-0.865565831794229,
1.62128617706663));
#28356=CARTESIAN_POINT('Ctrl Pts',(-6.69518164031139,-1.53656334674878,
0.601920948524818));
#28357=CARTESIAN_POINT('Ctrl Pts',(-6.65505912450737,-1.55783959376381,
0.0440901075324884));
#28358=CARTESIAN_POINT('Ctrl Pts',(-6.65194377439629,-1.55757973858287,
0.000756704723131364));
#28359=CARTESIAN_POINT('Origin',(-16.9400562256037,0.,0.));
#28360=CARTESIAN_POINT('',(-8.1900562256037,-1.55665418971026,0.00122204596489902));
#28361=CARTESIAN_POINT('',(-8.05194377439629,-1.55298816336082,0.000219416486716834));
#28362=CARTESIAN_POINT('',(-16.9400562256037,-1.5555,-7.70311135908521E-14));
#28363=CARTESIAN_POINT('Ctrl Pts',(-8.1900562256037,-1.55665418971026,0.00122204596489912));
#28364=CARTESIAN_POINT('Ctrl Pts',(-8.15888354994909,-1.5529084750837,-0.433054190629925));
#28365=CARTESIAN_POINT('Ctrl Pts',(-8.09070370860153,-1.1376911274873,-1.38916802661491));
#28366=CARTESIAN_POINT('Ctrl Pts',(-7.98551670156104,0.481614916815858,
-1.77364606800387));
#28367=CARTESIAN_POINT('Ctrl Pts',(-7.87449520448221,1.75075787078272,-0.559124476782657));
#28368=CARTESIAN_POINT('Ctrl Pts',(-7.76347370740338,1.42048470756065,1.16618887759722));
#28369=CARTESIAN_POINT('Ctrl Pts',(-7.65245221032457,-0.207481399618984,
1.82612287961606));
#28370=CARTESIAN_POINT('Ctrl Pts',(-7.56131304972465,-1.3883013990334,0.998368235695849));
#28371=CARTESIAN_POINT('Ctrl Pts',(-7.50718105481771,-1.55345099736004,
0.240306922105225));
#28372=CARTESIAN_POINT('Ctrl Pts',(-7.4900562256037,-1.5530180908049,0.000313254609165155));
#28373=CARTESIAN_POINT('Ctrl Pts',(-8.05194377439629,-1.55298816336082,
0.00021941648671699));
#28374=CARTESIAN_POINT('Ctrl Pts',(-8.03247844615601,-1.55264386792659,
-0.272587956900562));
#28375=CARTESIAN_POINT('Ctrl Pts',(-7.97600595222279,-1.35426737168086,
-1.06452050752492));
#28376=CARTESIAN_POINT('Ctrl Pts',(-7.88252629259662,-0.0920545910400277,
-1.83556504362701));
#28377=CARTESIAN_POINT('Ctrl Pts',(-7.77150479551779,1.49111460364442,-1.07440696010184));
#28378=CARTESIAN_POINT('Ctrl Pts',(-7.66048329843897,1.71206645837288,0.668282514533717));
#28379=CARTESIAN_POINT('Ctrl Pts',(-7.54946180136013,0.368948984659062,
1.80045819830287));
#28380=CARTESIAN_POINT('Ctrl Pts',(-7.44661529334591,-1.18750584841491,
1.32556192353867));
#28381=CARTESIAN_POINT('Ctrl Pts',(-7.38077595102464,-1.55198541440245,
0.40091181575136));
#28382=CARTESIAN_POINT('Ctrl Pts',(-7.3519437743963,-1.55568612057705,-0.00140331110564832));
#28383=CARTESIAN_POINT('Origin',(-16.9400562256037,0.,0.));
#28384=CARTESIAN_POINT('',(-8.8900562256037,-1.55680109303704,-0.00117256108906006));
#28385=CARTESIAN_POINT('',(-8.7519437743963,-1.55648790187904,0.0012702340526393));
#28386=CARTESIAN_POINT('',(-16.9400562256037,-1.5555,-7.70311135908521E-14));
#28387=CARTESIAN_POINT('Ctrl Pts',(-8.8900562256037,-1.55680109303704,-0.00117256108905984));
#28388=CARTESIAN_POINT('Ctrl Pts',(-8.88460037646635,-1.5574388429621,-0.0771610424262627));
#28389=CARTESIAN_POINT('Ctrl Pts',(-8.84213736163605,-1.51787106717481,
-0.667914644327412));
#28390=CARTESIAN_POINT('Ctrl Pts',(-8.7626671811128,-0.761733736392313,
-1.67258333648488));
#28391=CARTESIAN_POINT('Ctrl Pts',(-8.651645684034,0.990492616380764,-1.54812715225214));
#28392=CARTESIAN_POINT('Ctrl Pts',(-8.54062418695516,1.83784806665277,-0.00936944746539623));
#28393=CARTESIAN_POINT('Ctrl Pts',(-8.42960268987634,1.00622559096247,1.53794777633616));
#28394=CARTESIAN_POINT('Ctrl Pts',(-8.31858119279751,-0.744640747383609,
1.68026291394564));
#28395=CARTESIAN_POINT('Ctrl Pts',(-8.2387323713733,-1.51463350220016,0.678606070894573));
#28396=CARTESIAN_POINT('Ctrl Pts',(-8.19589071564203,-1.55735526314127,
0.0825041407189418));
#28397=CARTESIAN_POINT('Ctrl Pts',(-8.1900562256037,-1.55665418971026,0.00122204596489912));
#28398=CARTESIAN_POINT('Ctrl Pts',(-8.7519437743963,-1.55648790187904,0.00127023405263929));
#28399=CARTESIAN_POINT('Ctrl Pts',(-8.72118810698033,-1.55270169329837,
-0.427315239145853));
#28400=CARTESIAN_POINT('Ctrl Pts',(-8.65342527387141,-1.14681610862558,
-1.37790157034533));
#28401=CARTESIAN_POINT('Ctrl Pts',(-8.54865527506958,0.461668379793908,
-1.77894220935235));
#28402=CARTESIAN_POINT('Ctrl Pts',(-8.43763377799074,1.74436906067446,-0.578748354018101));
#28403=CARTESIAN_POINT('Ctrl Pts',(-8.32661228091193,1.43349016294594,1.15016478378281));
#28404=CARTESIAN_POINT('Ctrl Pts',(-8.21559078383309,-0.186962896184165,
1.82833748322551));
#28405=CARTESIAN_POINT('Ctrl Pts',(-8.12403461499455,-1.38244825556081,
1.01016791192593));
#28406=CARTESIAN_POINT('Ctrl Pts',(-8.06948561184895,-1.55329843681054,
0.246068987620239));
#28407=CARTESIAN_POINT('Ctrl Pts',(-8.05194377439629,-1.55298816336082,
0.00021941648671699));
#28408=CARTESIAN_POINT('Origin',(-16.9400562256037,0.,0.));
#28409=CARTESIAN_POINT('',(-9.5900562256037,-1.55305431186606,-0.000397270594051011));
#28410=CARTESIAN_POINT('',(-9.45194377439629,-1.55695751420806,-0.00111193227041603));
#28411=CARTESIAN_POINT('',(-16.9400562256037,-1.5555,-7.70311135908521E-14));
#28412=CARTESIAN_POINT('Ctrl Pts',(-9.5900562256037,-1.55305431186606,-0.000397270594050692));
#28413=CARTESIAN_POINT('Ctrl Pts',(-9.57331003729067,-1.5535918950784,-0.235070859271372));
#28414=CARTESIAN_POINT('Ctrl Pts',(-9.51955668328469,-1.39353800000331,
-0.98765021615145));
#28415=CARTESIAN_POINT('Ctrl Pts',(-9.42879616358577,-0.226089474720918,
-1.82391251217418));
#28416=CARTESIAN_POINT('Ctrl Pts',(-9.31777466650694,1.40852059510137,-1.18061129751514));
#28417=CARTESIAN_POINT('Ctrl Pts',(-9.20675316942812,1.75636761288009,0.541244964014445));
#28418=CARTESIAN_POINT('Ctrl Pts',(-9.09573167234929,0.499673697483888,
1.76864340631115));
#28419=CARTESIAN_POINT('Ctrl Pts',(-8.99016602440781,-1.12931106646732,
1.3993710384868));
#28420=CARTESIAN_POINT('Ctrl Pts',(-8.92160754215929,-1.55311296873919,
0.438270790237053));
#28421=CARTESIAN_POINT('Ctrl Pts',(-8.8900562256037,-1.55680109303704,-0.00117256108905984));
#28422=CARTESIAN_POINT('Ctrl Pts',(-9.4519437743963,-1.55695751420806,-0.00111193227041606));
#28423=CARTESIAN_POINT('Ctrl Pts',(-9.44690493349759,-1.55752501833762,
-0.0712739806210275));
#28424=CARTESIAN_POINT('Ctrl Pts',(-9.40485892690594,-1.52136701702691,
-0.656144510346978));
#28425=CARTESIAN_POINT('Ctrl Pts',(-9.32580575462134,-0.780467016280449,
-1.66392437136285));
#28426=CARTESIAN_POINT('Ctrl Pts',(-9.21478425754254,0.973046316719188,
-1.5591516740318));
#28427=CARTESIAN_POINT('Ctrl Pts',(-9.10376276046368,1.83762692652266,-0.0300059333434424));
#28428=CARTESIAN_POINT('Ctrl Pts',(-8.99274126338489,1.02343163435251,1.5265519208083));
#28429=CARTESIAN_POINT('Ctrl Pts',(-8.88171976630603,-0.725726212115684,
1.68851844590611));
#28430=CARTESIAN_POINT('Ctrl Pts',(-8.80145393664319,-1.51099768765163,
0.690385345643029));
#28431=CARTESIAN_POINT('Ctrl Pts',(-8.75819527267327,-1.55725749910801,
0.088385929218701));
#28432=CARTESIAN_POINT('Ctrl Pts',(-8.7519437743963,-1.55648790187904,0.00127023405263929));
#28433=CARTESIAN_POINT('Origin',(-16.9400562256037,0.,0.));
#28434=CARTESIAN_POINT('',(-10.2900562256037,-1.55535099785736,0.00141466667608078));
#28435=CARTESIAN_POINT('',(-10.1519437743963,-1.55310404192406,-0.000488110324520369));
#28436=CARTESIAN_POINT('',(-16.9400562256037,-1.5555,-7.70311135908521E-14));
#28437=CARTESIAN_POINT('Ctrl Pts',(-10.2900562256037,-1.55535099785736,
0.00141466667608059));
#28438=CARTESIAN_POINT('Ctrl Pts',(-10.262019698115,-1.5517955612436,-0.390013984173206));
#28439=CARTESIAN_POINT('Ctrl Pts',(-10.1969760049333,-1.20367189210361,
-1.30374819544608));
#28440=CARTESIAN_POINT('Ctrl Pts',(-10.0949251460587,0.330292110303061,
-1.80794923173099));
#28441=CARTESIAN_POINT('Ctrl Pts',(-9.98390364897991,1.69735659323361,-0.704807702888898));
#28442=CARTESIAN_POINT('Ctrl Pts',(-9.87288215190106,1.51379003966279,1.04221543764369));
#28443=CARTESIAN_POINT('Ctrl Pts',(-9.76186065482225,-0.0527091443318308,
1.83711595952703));
#28444=CARTESIAN_POINT('Ctrl Pts',(-9.66758534605645,-1.34203220347939,
1.08695838544496));
#28445=CARTESIAN_POINT('Ctrl Pts',(-9.61031720298361,-1.55240389750898,
0.283530999109612));
#28446=CARTESIAN_POINT('Ctrl Pts',(-9.5900562256037,-1.55305431186606,-0.000397270594050692));
#28447=CARTESIAN_POINT('Ctrl Pts',(-10.1519437743963,-1.55310404192406,
-0.000488110324520508));
#28448=CARTESIAN_POINT('Ctrl Pts',(-10.1356145943219,-1.5537492772768,-0.22929960521096));
#28449=CARTESIAN_POINT('Ctrl Pts',(-10.0822782485546,-1.3992198808917,-0.975842246865478));
#28450=CARTESIAN_POINT('Ctrl Pts',(-9.99193473709432,-0.246555808489883,
-1.82125871594808));
#28451=CARTESIAN_POINT('Ctrl Pts',(-9.88091324001547,1.39517473801909,-1.19635301124305));
#28452=CARTESIAN_POINT('Ctrl Pts',(-9.76989174293666,1.76233442608894,0.521488684190485));
#28453=CARTESIAN_POINT('Ctrl Pts',(-9.65887024585783,0.519502160386579,
1.76292103693575));
#28454=CARTESIAN_POINT('Ctrl Pts',(-9.5528875896777,-1.1199772158385,1.41057736623951));
#28455=CARTESIAN_POINT('Ctrl Pts',(-9.48391209919053,-1.55335705197859,
0.444022811014936));
#28456=CARTESIAN_POINT('Ctrl Pts',(-9.4519437743963,-1.55695751420806,-0.00111193227041606));
#28457=CARTESIAN_POINT('Origin',(-16.9400562256037,0.,0.));
#28458=CARTESIAN_POINT('',(-10.9900562256037,-1.5577736303666,-0.000579010970803218));
#28459=CARTESIAN_POINT('',(-10.8519437743963,-1.55517737544971,0.00141046793165706));
#28460=CARTESIAN_POINT('',(-16.9400562256037,-1.5555,-7.70311135908521E-14));
#28461=CARTESIAN_POINT('Ctrl Pts',(-10.9900562256037,-1.5577736303666,-0.000579010970803324));
#28462=CARTESIAN_POINT('Ctrl Pts',(-10.9877365246322,-1.55792790669674,
-0.0328345769997972));
#28463=CARTESIAN_POINT('Ctrl Pts',(-10.9484096579678,-1.54241106195977,
-0.579525553204954));
#28464=CARTESIAN_POINT('Ctrl Pts',(-10.8720756256105,-0.900100912087758,
-1.60237063462356));
#28465=CARTESIAN_POINT('Ctrl Pts',(-10.7610541285317,0.85637872338898,-1.62615767524916));
#28466=CARTESIAN_POINT('Ctrl Pts',(-10.6500326314529,1.83050806619295,-0.164357908990289));
#28467=CARTESIAN_POINT('Ctrl Pts',(-10.539011134374,1.13236498768008,1.44759208250163));
#28468=CARTESIAN_POINT('Ctrl Pts',(-10.4279896372952,-0.600257410937894,
1.73708501325043));
#28469=CARTESIAN_POINT('Ctrl Pts',(-10.3450046677051,-1.48544841640631,
0.767296463912538));
#28470=CARTESIAN_POINT('Ctrl Pts',(-10.2990268638079,-1.5564886043435,0.126657167229999));
#28471=CARTESIAN_POINT('Ctrl Pts',(-10.2900562256037,-1.55535099785736,
0.00141466667608059));
#28472=CARTESIAN_POINT('Ctrl Pts',(-10.8519437743963,-1.55517737544971,
0.00141046793165704));
#28473=CARTESIAN_POINT('Ctrl Pts',(-10.8243242551462,-1.5517190272114,-0.384305966949585));
#28474=CARTESIAN_POINT('Ctrl Pts',(-10.7596975702032,-1.21199099487677,
-1.29228056265986));
#28475=CARTESIAN_POINT('Ctrl Pts',(-10.6580637195673,0.309969930699919,
-1.81154401524745));
#28476=CARTESIAN_POINT('Ctrl Pts',(-10.5470422224884,1.68933528416089,-0.723822750959111));
#28477=CARTESIAN_POINT('Ctrl Pts',(-10.4360207254096,1.52539751963279,1.02515144452665));
#28478=CARTESIAN_POINT('Ctrl Pts',(-10.3249992283308,-0.0320769633279623,
1.83759194206456));
#28479=CARTESIAN_POINT('Ctrl Pts',(-10.2303069113264,-1.33548212909013,
1.09870548750621));
#28480=CARTESIAN_POINT('Ctrl Pts',(-10.1726217600148,-1.55228696676881,
0.289260718402204));
#28481=CARTESIAN_POINT('Ctrl Pts',(-10.1519437743963,-1.55310404192406,
-0.000488110324520508));
#28482=CARTESIAN_POINT('Origin',(-16.9400562256037,0.,0.));
#28483=CARTESIAN_POINT('',(-11.6900562256037,-1.55366781884501,-0.00100983995776636));
#28484=CARTESIAN_POINT('',(-11.5519437743963,-1.55785653804749,-0.000480323856083265));
#28485=CARTESIAN_POINT('',(-16.9400562256037,-1.5555,-7.70311135908521E-14));
#28486=CARTESIAN_POINT('Ctrl Pts',(-11.6900562256037,-1.55366781884501,
-0.00100983995776658));
#28487=CARTESIAN_POINT('Ctrl Pts',(-11.6764461854566,-1.55480484065087,
-0.191546334115928));
#28488=CARTESIAN_POINT('Ctrl Pts',(-11.6258289796165,-1.43412071110437,
-0.898781982870385));
#28489=CARTESIAN_POINT('Ctrl Pts',(-11.5382046080835,-0.379130133977537,
-1.79834191525306));
#28490=CARTESIAN_POINT('Ctrl Pts',(-11.4271831110046,1.30391677723258,-1.2952120832884));
#28491=CARTESIAN_POINT('Ctrl Pts',(-11.3161616139258,1.79576212723163,0.391167080728389));
#28492=CARTESIAN_POINT('Ctrl Pts',(-11.205140116847,0.647077432006542,1.72019304138606));
#28493=CARTESIAN_POINT('Ctrl Pts',(-11.0964383207396,-1.05639680161046,
1.48279173541205));
#28494=CARTESIAN_POINT('Ctrl Pts',(-11.0247436903252,-1.55546667148486,
0.481752040517312));
#28495=CARTESIAN_POINT('Ctrl Pts',(-10.9900562256037,-1.5577736303666,-0.000579010970803324));
#28496=CARTESIAN_POINT('Ctrl Pts',(-11.5519437743963,-1.55785653804749,
-0.000480323856082957));
#28497=CARTESIAN_POINT('Ctrl Pts',(-11.5500410816635,-1.55796398188818,
-0.026933615327131));
#28498=CARTESIAN_POINT('Ctrl Pts',(-11.5111312232377,-1.54537528569271,
-0.567796152963855));
#28499=CARTESIAN_POINT('Ctrl Pts',(-11.435214199119,-0.918037049911427,
-1.59216238245569));
#28500=CARTESIAN_POINT('Ctrl Pts',(-11.3241927020402,0.838064683925275,
-1.63567131865609));
#28501=CARTESIAN_POINT('Ctrl Pts',(-11.2131712049614,1.82854703367336,-0.184902197827091));
#28502=CARTESIAN_POINT('Ctrl Pts',(-11.1021497078826,1.14854847598013,1.43478551548331));
#28503=CARTESIAN_POINT('Ctrl Pts',(-10.9911282108037,-0.580713931678918,
1.74371568974732));
#28504=CARTESIAN_POINT('Ctrl Pts',(-10.907726232975,-1.4812414118026,0.779105032812509));
#28505=CARTESIAN_POINT('Ctrl Pts',(-10.8613314208392,-1.55635283944833,
0.132512297948512));
#28506=CARTESIAN_POINT('Ctrl Pts',(-10.8519437743963,-1.55517737544971,
0.00141046793165704));
#28507=CARTESIAN_POINT('Origin',(-16.9400562256037,0.,0.));
#28508=CARTESIAN_POINT('',(-12.3900562256037,-1.55413552921628,0.00122121428746227));
#28509=CARTESIAN_POINT('',(-12.2519437743963,-1.55378767035869,-0.0010750654722666));
#28510=CARTESIAN_POINT('',(-16.9400562256037,-1.5555,-7.70311135908521E-14));
#28511=CARTESIAN_POINT('Ctrl Pts',(-12.3900562256037,-1.55413552921628,
0.0012212142874622));
#28512=CARTESIAN_POINT('Ctrl Pts',(-12.3651558462809,-1.55156996285741,
-0.347112742422888));
#28513=CARTESIAN_POINT('Ctrl Pts',(-12.3032483012651,-1.2636873551123,-1.21698840048794));
#28514=CARTESIAN_POINT('Ctrl Pts',(-12.2043335905564,0.176615125299183,
-1.82936611977922));
#28515=CARTESIAN_POINT('Ctrl Pts',(-12.0933120934776,1.63185729621746,-0.845467366266227));
#28516=CARTESIAN_POINT('Ctrl Pts',(-11.9822905963988,1.59630573484127,0.910813539398446));
#28517=CARTESIAN_POINT('Ctrl Pts',(-11.8712690993199,0.10243879880857,1.83501487600212));
#28518=CARTESIAN_POINT('Ctrl Pts',(-11.7738576423882,-1.29040741479283,
1.17503675398003));
#28519=CARTESIAN_POINT('Ctrl Pts',(-11.7134533511495,-1.55171315584237,
0.326542924521853));
#28520=CARTESIAN_POINT('Ctrl Pts',(-11.6900562256037,-1.55366781884501,
-0.00100983995776658));
#28521=CARTESIAN_POINT('Ctrl Pts',(-12.2519437743963,-1.55378767035869,
-0.00107506547226662));
#28522=CARTESIAN_POINT('Ctrl Pts',(-12.2387507424878,-1.55496678448482,
-0.185737759807948));
#28523=CARTESIAN_POINT('Ctrl Pts',(-12.1885505448864,-1.43915025335468,
-0.886958792124525));
#28524=CARTESIAN_POINT('Ctrl Pts',(-12.101343181592,-0.399299683385937,
-1.79397124836776));
#28525=CARTESIAN_POINT('Ctrl Pts',(-11.9903216845132,1.28929067374477,-1.30977197851782));
#28526=CARTESIAN_POINT('Ctrl Pts',(-11.8793001874343,1.80004124060888,0.370977909346943));
#28527=CARTESIAN_POINT('Ctrl Pts',(-11.7682786903555,0.666352550691795,
1.71281854126591));
#28528=CARTESIAN_POINT('Ctrl Pts',(-11.6591598860095,-1.04622477450308,
1.49372311766702));
#28529=CARTESIAN_POINT('Ctrl Pts',(-11.5870482473564,-1.55587421093005,
0.487580012496977));
#28530=CARTESIAN_POINT('Ctrl Pts',(-11.5519437743963,-1.55785653804749,
-0.000480323856082957));
#28531=CARTESIAN_POINT('Origin',(-16.9400562256037,0.,0.));
#28532=CARTESIAN_POINT('',(-13.0900562256037,-1.55800332081628,0.000210157868350831));
#28533=CARTESIAN_POINT('',(-12.9519437743963,-1.55399622131086,0.00116937500724938));
#28534=CARTESIAN_POINT('',(-16.9400562256037,-1.5555,-7.70311135908521E-14));
#28535=CARTESIAN_POINT('Ctrl Pts',(-13.0900562256037,-1.55800332081628,
0.00021015786835074));
#28536=CARTESIAN_POINT('Ctrl Pts',(-13.0538655071052,-1.55704751416205,
-0.502825518255894));
#28537=CARTESIAN_POINT('Ctrl Pts',(-12.9806676229138,-1.0191962748975,-1.52200078717984));
#28538=CARTESIAN_POINT('Ctrl Pts',(-12.8704625730293,0.716160935289581,
-1.69259765416285));
#28539=CARTESIAN_POINT('Ctrl Pts',(-12.7594410759505,1.81012100052783,-0.318174898587703));
#28540=CARTESIAN_POINT('Ctrl Pts',(-12.6484195788717,1.25043337930754,1.3469185818581));
#28541=CARTESIAN_POINT('Ctrl Pts',(-12.5373980817929,-0.451595700759593,
1.78152592625865));
#28542=CARTESIAN_POINT('Ctrl Pts',(-12.4512769640369,-1.45185853317557,
0.856161387294219));
#28543=CARTESIAN_POINT('Ctrl Pts',(-12.4021630119738,-1.55538293044751,
0.170584288828434));
#28544=CARTESIAN_POINT('Ctrl Pts',(-12.3900562256037,-1.55413552921628,
0.0012212142874622));
#28545=CARTESIAN_POINT('Ctrl Pts',(-12.9519437743963,-1.55399622131086,
0.00116937500724928));
#28546=CARTESIAN_POINT('Ctrl Pts',(-12.9274604033121,-1.55159520168044,
-0.341408350569593));
#28547=CARTESIAN_POINT('Ctrl Pts',(-12.865969866535,-1.2712304187298,-1.20537147389457));
#28548=CARTESIAN_POINT('Ctrl Pts',(-12.767472164065,0.156062150750201,-1.83123392346586));
#28549=CARTESIAN_POINT('Ctrl Pts',(-12.6564506669861,1.62226066059323,-0.863738054150705));
#28550=CARTESIAN_POINT('Ctrl Pts',(-12.5454291699073,1.60643250632205,0.892831271683784));
#28551=CARTESIAN_POINT('Ctrl Pts',(-12.4344076728285,0.123037600173064,
1.8337488448793));
#28552=CARTESIAN_POINT('Ctrl Pts',(-12.3365792076581,-1.28312558209438,
1.18669436910945));
#28553=CARTESIAN_POINT('Ctrl Pts',(-12.2757579081807,-1.55165930579917,
0.332251052315397));
#28554=CARTESIAN_POINT('Ctrl Pts',(-12.2519437743963,-1.55378767035869,
-0.00107506547226662));
#28555=CARTESIAN_POINT('Origin',(-16.9400562256037,0.,0.));
#28556=CARTESIAN_POINT('',(-13.7900562256037,-1.55473841727083,-0.00136756133992672));
#28557=CARTESIAN_POINT('',(-13.6519437743963,-1.55795954537968,0.000315683116621389));
#28558=CARTESIAN_POINT('',(-16.9400562256037,-1.5555,-7.70311135908521E-14));
#28559=CARTESIAN_POINT('Ctrl Pts',(-13.7900562256037,-1.55473841727083,
-0.00136756133992656));
#28560=CARTESIAN_POINT('Ctrl Pts',(-13.7795823336225,-1.55598127536203,
-0.147744259734356));
#28561=CARTESIAN_POINT('Ctrl Pts',(-13.7321012759483,-1.46991308354017,
-0.809877587435659));
#28562=CARTESIAN_POINT('Ctrl Pts',(-13.6476130525811,-0.529468511212632,
-1.75995347711011));
#28563=CARTESIAN_POINT('Ctrl Pts',(-13.5365915555023,1.19001920390447,-1.40058118296215));
#28564=CARTESIAN_POINT('Ctrl Pts',(-13.4255700584235,1.82235723230149,0.238301140323824));
#28565=CARTESIAN_POINT('Ctrl Pts',(-13.3145485613446,0.789869078999073,
1.65948188258691));
#28566=CARTESIAN_POINT('Ctrl Pts',(-13.2035270642659,-0.964209049677692,
1.56463229551752));
#28567=CARTESIAN_POINT('Ctrl Pts',(-13.1286962856855,-1.5527764949361,0.537270179800524));
#28568=CARTESIAN_POINT('Ctrl Pts',(-13.0908726727981,-1.55802488340729,
0.0115584284612541));
#28569=CARTESIAN_POINT('Ctrl Pts',(-13.0900562256037,-1.55800332081628,
0.00021015786835074));
#28570=CARTESIAN_POINT('Ctrl Pts',(-13.6519437743963,-1.55795954537968,
0.000315683116621417));
#28571=CARTESIAN_POINT('Ctrl Pts',(-13.6161700641364,-1.55657771788537,
-0.496961205609469));
#28572=CARTESIAN_POINT('Ctrl Pts',(-13.5433891881836,-1.02966362241915,
-1.51117950611935));
#28573=CARTESIAN_POINT('Ctrl Pts',(-13.4336011465379,0.697109689533605,
-1.70053261271694));
#28574=CARTESIAN_POINT('Ctrl Pts',(-13.3225796494591,1.8064340535295,-0.338480558245879));
#28575=CARTESIAN_POINT('Ctrl Pts',(-13.2115581523802,1.26547896337724,1.33279258226153));
#28576=CARTESIAN_POINT('Ctrl Pts',(-13.1005366553014,-0.431562574783867,
1.78648448709609));
#28577=CARTESIAN_POINT('Ctrl Pts',(-13.0139985293068,-1.44704656389406,
0.867984154568371));
#28578=CARTESIAN_POINT('Ctrl Pts',(-12.9644675690051,-1.55522439681821,
0.176405581570162));
#28579=CARTESIAN_POINT('Ctrl Pts',(-12.9519437743963,-1.55399622131086,
0.00116937500724928));
#28580=CARTESIAN_POINT('Origin',(-16.9400562256037,0.,0.));
#28581=CARTESIAN_POINT('',(-14.4900562256037,-1.55328082746597,0.000715383538183075));
#28582=CARTESIAN_POINT('',(-14.3519437743963,-1.55490416069612,-0.00138938706337133));
#28583=CARTESIAN_POINT('',(-16.9400562256037,-1.5555,-7.70311135908521E-14));
#28584=CARTESIAN_POINT('Ctrl Pts',(-14.4900562256037,-1.55328082746597,
0.000715383538183074));
#28585=CARTESIAN_POINT('Ctrl Pts',(-14.4682919944468,-1.55201539840468,
-0.304168296634556));
#28586=CARTESIAN_POINT('Ctrl Pts',(-14.4095205975969,-1.31797175976879,
-1.129261225486));
#28587=CARTESIAN_POINT('Ctrl Pts',(-14.3137420350541,0.0216796534424384,
-1.83774207162163));
#28588=CARTESIAN_POINT('Ctrl Pts',(-14.2027205379753,1.55472664688603,-0.980101962297276));
#28589=CARTESIAN_POINT('Ctrl Pts',(-14.0916990408964,1.66744375345186,0.772920313447068));
#28590=CARTESIAN_POINT('Ctrl Pts',(-13.9806775438176,0.256856552130983,
1.81983431302347));
#28591=CARTESIAN_POINT('Ctrl Pts',(-13.88012993872,-1.23316965064986,1.26230497981326));
#28592=CARTESIAN_POINT('Ctrl Pts',(-13.8165894993154,-1.55158991297295,
0.369445218710443));
#28593=CARTESIAN_POINT('Ctrl Pts',(-13.7900562256037,-1.55473841727083,
-0.00136756133992656));
#28594=CARTESIAN_POINT('Ctrl Pts',(-14.3519437743963,-1.55490416069612,
-0.00138938706337152));
#28595=CARTESIAN_POINT('Ctrl Pts',(-14.3418868906537,-1.55612679718045,
-0.141900236675545));
#28596=CARTESIAN_POINT('Ctrl Pts',(-14.2948228412182,-1.47432573136466,
-0.798062339120933));
#28597=CARTESIAN_POINT('Ctrl Pts',(-14.2107516260897,-0.549197426397097,
-1.75389685400554));
#28598=CARTESIAN_POINT('Ctrl Pts',(-14.0997301290109,1.17421705517224,-1.41385560804608));
#28599=CARTESIAN_POINT('Ctrl Pts',(-13.988708631932,1.82491817106717,0.217823042681003));
#28600=CARTESIAN_POINT('Ctrl Pts',(-13.8776871348532,0.808453455731279,
1.65050777944339));
#28601=CARTESIAN_POINT('Ctrl Pts',(-13.7666656377744,-0.946579065961039,
1.57536065782744));
#28602=CARTESIAN_POINT('Ctrl Pts',(-13.6914178509554,-1.54998955482229,
0.54898434204543));
#28603=CARTESIAN_POINT('Ctrl Pts',(-13.6531772298294,-1.55800718993816,
0.0174614830823369));
#28604=CARTESIAN_POINT('Ctrl Pts',(-13.6519437743963,-1.55795954537968,
0.000315683116621417));
#28605=CARTESIAN_POINT('Origin',(-16.9400562256037,0.,0.));
#28606=CARTESIAN_POINT('',(-15.1900562256037,-1.55731346481242,0.00103325697183645));
#28607=CARTESIAN_POINT('',(-15.0519437743963,-1.55320111767851,0.000640865722738582));
#28608=CARTESIAN_POINT('',(-16.9400562256037,-1.5555,-7.70311135908521E-14));
#28609=CARTESIAN_POINT('Ctrl Pts',(-15.1900562256037,-1.55731346481242,
0.00103325697183652));
#28610=CARTESIAN_POINT('Ctrl Pts',(-15.1570016552711,-1.55406616181334,
-0.458910165558249));
#28611=CARTESIAN_POINT('Ctrl Pts',(-15.0869399192455,-1.09517591543371,
-1.43978275398639));
#28612=CARTESIAN_POINT('Ctrl Pts',(-14.979871017527,0.570855243925188,-1.74687800671557));
#28613=CARTESIAN_POINT('Ctrl Pts',(-14.8688495204482,1.77682346771718,-0.469774267555894));
#28614=CARTESIAN_POINT('Ctrl Pts',(-14.7578280233694,1.3595938034014,1.2366712040288));
#28615=CARTESIAN_POINT('Ctrl Pts',(-14.6468065262906,-0.299717618166574,
1.81325504017035));
#28616=CARTESIAN_POINT('Ctrl Pts',(-14.5575492603687,-1.41360466166464,
0.94507199546461));
#28617=CARTESIAN_POINT('Ctrl Pts',(-14.5052991601397,-1.55416709136393,
0.214245645391361));
#28618=CARTESIAN_POINT('Ctrl Pts',(-14.4900562256037,-1.55328082746597,
0.000715383538183074));
#28619=CARTESIAN_POINT('Ctrl Pts',(-15.0519437743963,-1.55320111767851,
0.000640865722738825));
#28620=CARTESIAN_POINT('Ctrl Pts',(-15.030596551478,-1.55211155703931,-0.298442301630793));
#28621=CARTESIAN_POINT('Ctrl Pts',(-14.9722421628668,-1.32477770343153,
-1.11755737738762));
#28622=CARTESIAN_POINT('Ctrl Pts',(-14.8768806085626,0.00104665412810624,
-1.83785829362665));
#28623=CARTESIAN_POINT('Ctrl Pts',(-14.7658591114838,1.54362083748287,-0.99750399698833));
#28624=CARTESIAN_POINT('Ctrl Pts',(-14.654837614405,1.67601881849698,0.754151058535186));
#28625=CARTESIAN_POINT('Ctrl Pts',(-14.5438161173262,0.277274533789786,
1.81683365360614));
#28626=CARTESIAN_POINT('Ctrl Pts',(-14.4428515039899,-1.22512254880408,
1.2738304268474));
#28627=CARTESIAN_POINT('Ctrl Pts',(-14.3788940563466,-1.55162775830162,
0.375149420687903));
#28628=CARTESIAN_POINT('Ctrl Pts',(-14.3519437743963,-1.55490416069612,
-0.00138938706337152));
#28629=CARTESIAN_POINT('Ctrl Pts',(-15.8760740822721,-0.685825729128752,
1.39614588036674));
#28630=CARTESIAN_POINT('Ctrl Pts',(-15.8390669165791,-1.14959124433326,
1.16833134674053));
#28631=CARTESIAN_POINT('Ctrl Pts',(-15.7650525851932,-1.82433082916238,
0.2182728247837));
#28632=CARTESIAN_POINT('Ctrl Pts',(-15.6540310881144,-1.17303546001366,
-1.41641485775535));
#28633=CARTESIAN_POINT('Ctrl Pts',(-15.5430095910356,0.551406182529313,
-1.75263860476265));
#28634=CARTESIAN_POINT('Ctrl Pts',(-15.4319880939568,1.77133009557791,-0.489978596140976));
#28635=CARTESIAN_POINT('Ctrl Pts',(-15.3209665968779,1.37345033995276,1.2214745163176));
#28636=CARTESIAN_POINT('Ctrl Pts',(-15.2099450997991,-0.279367108572254,
1.81642835228867));
#28637=CARTESIAN_POINT('Ctrl Pts',(-15.0989236027203,-1.67685487580139,
0.752294539512666));
#28638=CARTESIAN_POINT('Ctrl Pts',(-14.9879021056415,-1.54249996813387,
-0.999272066172348));
#28639=CARTESIAN_POINT('Ctrl Pts',(-14.8768806085626,0.00104665412810624,
-1.83785829362665));
#28640=CARTESIAN_POINT('Ctrl Pts',(-14.7658591114838,1.54362083748287,-0.99750399698833));
#28641=CARTESIAN_POINT('Ctrl Pts',(-14.654837614405,1.67601881849698,0.754151058535186));
#28642=CARTESIAN_POINT('Ctrl Pts',(-14.5438161173262,0.277274533789786,
1.81683365360614));
#28643=CARTESIAN_POINT('Ctrl Pts',(-14.4327946202473,-1.37477332540386,
1.21974295854618));
#28644=CARTESIAN_POINT('Ctrl Pts',(-14.3217731231685,-1.77088940801687,
-0.491655328889854));
#28645=CARTESIAN_POINT('Ctrl Pts',(-14.2107516260897,-0.549197426397097,
-1.75389685400554));
#28646=CARTESIAN_POINT('Ctrl Pts',(-14.0997301290109,1.17421705517224,-1.41385560804608));
#28647=CARTESIAN_POINT('Ctrl Pts',(-13.988708631932,1.82491817106717,0.217823042681003));
#28648=CARTESIAN_POINT('Ctrl Pts',(-13.8776871348532,0.808453455731279,
1.65050777944339));
#28649=CARTESIAN_POINT('Ctrl Pts',(-13.7666656377744,-0.946579065961039,
1.57536065782744));
#28650=CARTESIAN_POINT('Ctrl Pts',(-13.6556441406956,-1.83685821779324,
0.0610325963455999));
#28651=CARTESIAN_POINT('Ctrl Pts',(-13.5446226436167,-1.04906371273324,
-1.5090521467585));
#28652=CARTESIAN_POINT('Ctrl Pts',(-13.4336011465379,0.697109689533605,
-1.70053261271694));
#28653=CARTESIAN_POINT('Ctrl Pts',(-13.3225796494591,1.8064340535295,-0.338480558245879));
#28654=CARTESIAN_POINT('Ctrl Pts',(-13.2115581523802,1.26547896337724,1.33279258226153));
#28655=CARTESIAN_POINT('Ctrl Pts',(-13.1005366553014,-0.431562574783867,
1.78648448709609));
#28656=CARTESIAN_POINT('Ctrl Pts',(-12.9895151582226,-1.73434734663761,
0.60812199296339));
#28657=CARTESIAN_POINT('Ctrl Pts',(-12.8784936611437,-1.45270794093109,
-1.12579425965292));
#28658=CARTESIAN_POINT('Ctrl Pts',(-12.767472164065,0.156062150750201,-1.83123392346586));
#28659=CARTESIAN_POINT('Ctrl Pts',(-12.6564506669861,1.62226066059323,-0.863738054150705));
#28660=CARTESIAN_POINT('Ctrl Pts',(-12.5454291699073,1.60643250632205,0.892831271683784));
#28661=CARTESIAN_POINT('Ctrl Pts',(-12.4344076728285,0.123037600173064,
1.8337488448793));
#28662=CARTESIAN_POINT('Ctrl Pts',(-12.3233861757497,-1.47275909724666,
1.09943336250467));
#28663=CARTESIAN_POINT('Ctrl Pts',(-12.2123646786708,-1.72310724567287,
-0.639276541897258));
#28664=CARTESIAN_POINT('Ctrl Pts',(-12.101343181592,-0.399299683385937,
-1.79397124836776));
#28665=CARTESIAN_POINT('Ctrl Pts',(-11.9903216845132,1.28929067374477,-1.30977197851782));
#28666=CARTESIAN_POINT('Ctrl Pts',(-11.8793001874343,1.80004124060888,0.370977909346943));
#28667=CARTESIAN_POINT('Ctrl Pts',(-11.7682786903555,0.666352550691795,
1.71281854126591));
#28668=CARTESIAN_POINT('Ctrl Pts',(-11.6572571932767,-1.07608679920682,
1.4899027745761));
#28669=CARTESIAN_POINT('Ctrl Pts',(-11.5462356961979,-1.83546013017251,
-0.0941232578271086));
#28670=CARTESIAN_POINT('Ctrl Pts',(-11.435214199119,-0.918037049911427,
-1.59216238245569));
#28671=CARTESIAN_POINT('Ctrl Pts',(-11.3241927020402,0.838064683925275,
-1.63567131865609));
#28672=CARTESIAN_POINT('Ctrl Pts',(-11.2131712049614,1.82854703367336,-0.184902197827091));
#28673=CARTESIAN_POINT('Ctrl Pts',(-11.1021497078826,1.14854847598013,1.43478551548331));
#28674=CARTESIAN_POINT('Ctrl Pts',(-10.9911282108037,-0.580713931678918,
1.74371568974732));
#28675=CARTESIAN_POINT('Ctrl Pts',(-10.8801067137249,-1.77946139075276,
0.459663176616526));
#28676=CARTESIAN_POINT('Ctrl Pts',(-10.7690852166461,-1.35257044729127,
-1.24431758897447));
#28677=CARTESIAN_POINT('Ctrl Pts',(-10.6580637195673,0.309969930699919,
-1.81154401524745));
#28678=CARTESIAN_POINT('Ctrl Pts',(-10.5470422224884,1.68933528416089,-0.723822750959111));
#28679=CARTESIAN_POINT('Ctrl Pts',(-10.4360207254096,1.52539751963279,1.02515144452665));
#28680=CARTESIAN_POINT('Ctrl Pts',(-10.3249992283308,-0.0320769633279623,
1.83759194206456));
#28681=CARTESIAN_POINT('Ctrl Pts',(-10.213977731252,-1.56024733005802,0.971288497905627));
#28682=CARTESIAN_POINT('Ctrl Pts',(-10.1029562341731,-1.66304370981859,
-0.782341802762569));
#28683=CARTESIAN_POINT('Ctrl Pts',(-9.99193473709432,-0.246555808489883,
-1.82125871594808));
#28684=CARTESIAN_POINT('Ctrl Pts',(-9.88091324001547,1.39517473801909,-1.19635301124305));
#28685=CARTESIAN_POINT('Ctrl Pts',(-9.76989174293666,1.76233442608894,0.521488684190485));
#28686=CARTESIAN_POINT('Ctrl Pts',(-9.65887024585783,0.519502160386579,
1.76292103693575));
#28687=CARTESIAN_POINT('Ctrl Pts',(-9.547848748779,-1.19792464640174,1.39382553379547));
#28688=CARTESIAN_POINT('Ctrl Pts',(-9.43682725170018,-1.82097968505047,
-0.248608253584697));
#28689=CARTESIAN_POINT('Ctrl Pts',(-9.32580575462134,-0.780467016280449,
-1.66392437136285));
#28690=CARTESIAN_POINT('Ctrl Pts',(-9.21478425754254,0.973046316719188,
-1.5591516740318));
#28691=CARTESIAN_POINT('Ctrl Pts',(-9.10376276046368,1.83762692652266,-0.0300059333434424));
#28692=CARTESIAN_POINT('Ctrl Pts',(-8.99274126338489,1.02343163435251,1.5265519208083));
#28693=CARTESIAN_POINT('Ctrl Pts',(-8.88171976630603,-0.725726212115684,
1.68851844590611));
#28694=CARTESIAN_POINT('Ctrl Pts',(-8.77069826922724,-1.81189220820005,
0.307928080858025));
#28695=CARTESIAN_POINT('Ctrl Pts',(-8.65967677214839,-1.24279241981098,
-1.35397196366001));
#28696=CARTESIAN_POINT('Ctrl Pts',(-8.54865527506958,0.461668379793908,
-1.77894220935235));
#28697=CARTESIAN_POINT('Ctrl Pts',(-8.43763377799074,1.74436906067446,-0.578748354018101));
#28698=CARTESIAN_POINT('Ctrl Pts',(-8.32661228091193,1.43349016294594,1.15016478378281));
#28699=CARTESIAN_POINT('Ctrl Pts',(-8.21559078383309,-0.186962896184165,
1.82833748322551));
#28700=CARTESIAN_POINT('Ctrl Pts',(-8.10456928675427,-1.63661479859031,
0.836220711386745));
#28701=CARTESIAN_POINT('Ctrl Pts',(-7.99354778967544,-1.59112672180277,
-0.919830871563968));
#28702=CARTESIAN_POINT('Ctrl Pts',(-7.88252629259662,-0.0920545910400277,
-1.83556504362701));
#28703=CARTESIAN_POINT('Ctrl Pts',(-7.77150479551779,1.49111460364442,-1.07440696010184));
#28704=CARTESIAN_POINT('Ctrl Pts',(-7.66048329843897,1.71206645837288,0.668282514533717));
#28705=CARTESIAN_POINT('Ctrl Pts',(-7.54946180136013,0.368948984659062,
1.80045819830287));
#28706=CARTESIAN_POINT('Ctrl Pts',(-7.43844030428131,-1.31122420779922,
1.28781371090631));
#28707=CARTESIAN_POINT('Ctrl Pts',(-7.3274188072025,-1.7935200888365,-0.401321277852141));
#28708=CARTESIAN_POINT('Ctrl Pts',(-7.21639731012365,-0.637334153250706,
-1.723826631137));
#28709=CARTESIAN_POINT('Ctrl Pts',(-7.10537581304485,1.10109249863036,-1.47151907448626));
#28710=CARTESIAN_POINT('Ctrl Pts',(-6.994354315966,1.83360901398418,0.125104200380868));
#28711=CARTESIAN_POINT('Ctrl Pts',(-6.8833328188872,0.891020217215038,1.60743772807255));
#28712=CARTESIAN_POINT('Ctrl Pts',(-6.77231132180836,-0.865565831794229,
1.62128617706663));
#28713=CARTESIAN_POINT('Ctrl Pts',(-6.66128982472953,-1.83140864613746,
0.153998207683987));
#28714=CARTESIAN_POINT('Ctrl Pts',(-6.55026832765071,-1.12415630856125,
-1.45397581514925));
#28715=CARTESIAN_POINT('Ctrl Pts',(-6.43924683057189,0.610076257496618,
-1.73366087720635));
#28716=CARTESIAN_POINT('Ctrl Pts',(-6.32822533349305,1.78696973330201,-0.429548890557871));
#28717=CARTESIAN_POINT('Ctrl Pts',(-6.21720383641424,1.3313655119277,1.26698024876731));
#28718=CARTESIAN_POINT('Ctrl Pts',(-6.10618233933541,-0.340516238842866,
1.80605143010969));
#28719=CARTESIAN_POINT('Ctrl Pts',(-5.99516084225658,-1.70131718874498,
0.695192707382526));
#28720=CARTESIAN_POINT('Ctrl Pts',(-5.88413934517776,-1.50786887463394,
-1.05076378602764));
#28721=CARTESIAN_POINT('Ctrl Pts',(-5.77311784809893,0.0631027514921653,
-1.83678826212252));
#28722=CARTESIAN_POINT('Ctrl Pts',(-5.6620963510201,1.57642645299097,-0.944803003502463));
#28723=CARTESIAN_POINT('Ctrl Pts',(-5.55107485394128,1.64959562566877,0.810313117807789));
#28724=CARTESIAN_POINT('Ctrl Pts',(-5.44005335686245,0.215766101057041,
1.82516247680901));
#28725=CARTESIAN_POINT('Ctrl Pts',(-5.32903185978363,-1.41517793340943,
1.17262291206848));
#28726=CARTESIAN_POINT('Ctrl Pts',(-5.2180103627048,-1.75327706158784,-0.551173858620724));
#28727=CARTESIAN_POINT('Ctrl Pts',(-5.10698886562598,-0.489658649608892,
-1.77144220452719));
#28728=CARTESIAN_POINT('Ctrl Pts',(-4.99596736854715,1.22129057217261,-1.37339812706995));
#28729=CARTESIAN_POINT('Ctrl Pts',(-4.88494587146833,1.81652193399072,0.279322645783608));
#28730=CARTESIAN_POINT('Ctrl Pts',(-4.77392437438949,0.752257995551791,
1.67686641842616));
#28731=CARTESIAN_POINT('Ctrl Pts',(-4.66290287731068,-0.999236074733923,
1.54249808559599));
#28732=CARTESIAN_POINT('Ctrl Pts',(-4.55188138023185,-1.8378715998848,-0.00102929772714257));
#28733=CARTESIAN_POINT('Ctrl Pts',(-4.44085988315302,-0.997507700137877,
-1.5436163594892));
#28734=CARTESIAN_POINT('Ctrl Pts',(-4.3298383860742,0.754135777011385,-1.67602276444812));
#28735=CARTESIAN_POINT('Ctrl Pts',(-4.21881688899538,1.81683366297973,-0.277287789454163));
#28736=CARTESIAN_POINT('Ctrl Pts',(-4.10779539191654,1.21975146666773,1.37476522965911));
#28737=CARTESIAN_POINT('Ctrl Pts',(-3.99677389483772,-0.491642529871626,
1.77089262800929));
#28738=CARTESIAN_POINT('Ctrl Pts',(-3.88575239775889,-1.75389333002919,
0.549209672160667));
#28739=CARTESIAN_POINT('Ctrl Pts',(-3.77473090068007,-1.4138635940316,-1.17420731329451));
#28740=CARTESIAN_POINT('Ctrl Pts',(-3.66370940360124,0.217810325062528,
-1.82491965286328));
#28741=CARTESIAN_POINT('Ctrl Pts',(-3.55268790652242,1.65050222030251,-0.808464902075287));
#28742=CARTESIAN_POINT('Ctrl Pts',(-3.4416664094436,1.57536719290506,0.946568161661344));
#28743=CARTESIAN_POINT('Ctrl Pts',(-3.33064491236476,0.0610453305290268,
1.83685779108923));
#28744=CARTESIAN_POINT('Ctrl Pts',(-3.21962341528594,-1.50904488626973,
1.04907416721584));
#28745=CARTESIAN_POINT('Ctrl Pts',(-3.10860191820711,-1.70053743814524,
-0.697097911928709));
#28746=CARTESIAN_POINT('Ctrl Pts',(-2.99758042112829,-0.338493072017185,
-1.8064317083433));
#28747=CARTESIAN_POINT('Ctrl Pts',(-2.88655892404946,1.33278381758959,-1.26548819539577));
#28748=CARTESIAN_POINT('Ctrl Pts',(-2.77553742697064,1.78648747614462,0.431550201213581));
#28749=CARTESIAN_POINT('Ctrl Pts',(-2.66451592989181,0.608134005493306,
1.73434313370923));
#28750=CARTESIAN_POINT('Ctrl Pts',(-2.55349443281299,-1.12578419639739,
1.4527157399861));
#28751=CARTESIAN_POINT('Ctrl Pts',(-2.44247293573416,-1.83123500658462,
-0.156049469126138));
#28752=CARTESIAN_POINT('Ctrl Pts',(-2.33145143865534,-0.863749286419899,
-1.62225467335409));
#28753=CARTESIAN_POINT('Ctrl Pts',(-2.22042994157651,0.892820136543068,
-1.60643869907147));
#28754=CARTESIAN_POINT('Ctrl Pts',(-2.10940844449769,1.8337480082192,-0.123050285242695));
#28755=CARTESIAN_POINT('Ctrl Pts',(-1.99838694741886,1.09944353382152,1.47275145086502));
#28756=CARTESIAN_POINT('Ctrl Pts',(-1.88736545034003,-0.639264550272716,
1.72311173281902));
#28757=CARTESIAN_POINT('Ctrl Pts',(-1.77634395326121,-1.7939685901571,0.399311996552182));
#28758=CARTESIAN_POINT('Ctrl Pts',(-1.66532245618238,-1.30978070402824,
-1.28928138705521));
#28759=CARTESIAN_POINT('Ctrl Pts',(-1.55430095910356,0.370965051819814,
-1.80004421839588));
#28760=CARTESIAN_POINT('Ctrl Pts',(-1.44327946202473,1.71281466704483,-0.6663636376042));
#28761=CARTESIAN_POINT('Ctrl Pts',(-1.33225796494591,1.48990881738992,1.0760750010236));
#28762=CARTESIAN_POINT('Ctrl Pts',(-1.22123646786708,-0.0941078601541336,
1.83546359530854));
#28763=CARTESIAN_POINT('Ctrl Pts',(-1.11021497078826,-1.59216113185349,
0.918042724568974));
#28764=CARTESIAN_POINT('Ctrl Pts',(-0.999193473709428,-1.63566740285966,
-0.83804316724106));
#28765=CARTESIAN_POINT('Ctrl Pts',(-0.888171976630605,-0.184933360961542,
-1.82856513855231));
#28766=CARTESIAN_POINT('Ctrl Pts',(-0.777150479551777,1.43481276042301,
-1.14852152405029));
#28767=CARTESIAN_POINT('Ctrl Pts',(-0.666128982472953,1.74365272478113,
0.580631652352415));
#28768=CARTESIAN_POINT('Ctrl Pts',(-0.555107485394127,0.459803001478689,
1.7795918156029));
#28769=CARTESIAN_POINT('Ctrl Pts',(-0.444085988315302,-1.24455107634816,
1.35232464687182));
#28770=CARTESIAN_POINT('Ctrl Pts',(-0.333064491236475,-1.81108201871734,
-0.309471773373046));
#28771=CARTESIAN_POINT('Ctrl Pts',(-0.222042994157651,-0.72473494787801,
-1.69026698927826));
#28772=CARTESIAN_POINT('Ctrl Pts',(-0.111021497078823,1.0270020972766,-1.52351327282068));
#28773=CARTESIAN_POINT('Ctrl Pts',(-0.03700716569294,1.56427778786756,-0.489482550463674));
#28774=CARTESIAN_POINT('Ctrl Pts',(2.22044604925031E-15,1.55526325306019,
0.0271378643346999));
#28775=CARTESIAN_POINT('Ctrl Pts',(-15.7993827215147,-0.744392439309354,
1.51537102412034));
#28776=CARTESIAN_POINT('Ctrl Pts',(-15.7623755558218,-1.24776163131854,
1.26810206176809));
#28777=CARTESIAN_POINT('Ctrl Pts',(-15.6883612244359,-1.9801212149807,0.236912430628839));
#28778=CARTESIAN_POINT('Ctrl Pts',(-15.577339727357,-1.2732078870608,-1.53737088921693));
#28779=CARTESIAN_POINT('Ctrl Pts',(-15.4663182302782,0.598494013609971,
-1.90230676805375));
#28780=CARTESIAN_POINT('Ctrl Pts',(-15.3552967331994,1.92259443568029,-0.531820762767402));
#28781=CARTESIAN_POINT('Ctrl Pts',(-15.2442752361206,1.49073737744792,1.32578344051186));
#28782=CARTESIAN_POINT('Ctrl Pts',(-15.1332537390418,-0.303223916193815,
1.97154389892684));
#28783=CARTESIAN_POINT('Ctrl Pts',(-15.0222322419629,-1.82005141882225,
0.816537414043005));
#28784=CARTESIAN_POINT('Ctrl Pts',(-14.9112107448841,-1.67422315195502,
-1.08460581059957));
#28785=CARTESIAN_POINT('Ctrl Pts',(-14.8001892478053,0.00113603410668217,
-1.99480386954226));
#28786=CARTESIAN_POINT('Ctrl Pts',(-14.6891677507265,1.67543973895868,-1.08268675554397));
#28787=CARTESIAN_POINT('Ctrl Pts',(-14.5781462536476,1.81914396564604,0.818552472191297));
#28788=CARTESIAN_POINT('Ctrl Pts',(-14.4671247565688,0.300952644089851,
1.97198381131792));
#28789=CARTESIAN_POINT('Ctrl Pts',(-14.35610325949,-1.49217334044155,1.32390401479405));
#28790=CARTESIAN_POINT('Ctrl Pts',(-14.2450817624111,-1.92211611520528,
-0.533640681630147));
#28791=CARTESIAN_POINT('Ctrl Pts',(-14.1340602653324,-0.596096638744525,
-1.90367246663196));
#28792=CARTESIAN_POINT('Ctrl Pts',(-14.0230387682535,1.27449038560964,-1.53459309005752));
#28793=CARTESIAN_POINT('Ctrl Pts',(-13.9120172711747,1.98075871348017,0.236424238975518));
#28794=CARTESIAN_POINT('Ctrl Pts',(-13.8009957740958,0.877492071848058,
1.79145438827402));
#28795=CARTESIAN_POINT('Ctrl Pts',(-13.689974277017,-1.02741304384284,1.70989001004951));
#28796=CARTESIAN_POINT('Ctrl Pts',(-13.5789527799382,-1.99371839132599,
0.0662445302669022));
#28797=CARTESIAN_POINT('Ctrl Pts',(-13.4679312828594,-1.13864945997941,
-1.63791902353622));
#28798=CARTESIAN_POINT('Ctrl Pts',(-13.3569097857806,0.756640003747492,
-1.84575113755733));
#28799=CARTESIAN_POINT('Ctrl Pts',(-13.2458882887017,1.96069612796034,-0.367385412518035));
#28800=CARTESIAN_POINT('Ctrl Pts',(-13.1348667916229,1.37354568724006,1.44660761366219));
#28801=CARTESIAN_POINT('Ctrl Pts',(-13.023845294544,-0.468416252283351,
1.93904295020716));
#28802=CARTESIAN_POINT('Ctrl Pts',(-12.9128237974653,-1.88245351135101,
0.660053122117134));
#28803=CARTESIAN_POINT('Ctrl Pts',(-12.8018023003864,-1.57676325314819,
-1.22193248154763));
#28804=CARTESIAN_POINT('Ctrl Pts',(-12.6907808033076,0.16938921966136,-1.98761380528331));
#28805=CARTESIAN_POINT('Ctrl Pts',(-12.5797593062288,1.76079508108961,-0.937497748692457));
#28806=CARTESIAN_POINT('Ctrl Pts',(-12.4687378091499,1.74361526722837,0.969075407924211));
#28807=CARTESIAN_POINT('Ctrl Pts',(-12.3577163120711,0.133544507634545,
1.99034349069188));
#28808=CARTESIAN_POINT('Ctrl Pts',(-12.2466948149923,-1.59852669614364,
1.19332047167817));
#28809=CARTESIAN_POINT('Ctrl Pts',(-12.1356733179135,-1.87025355176966,
-0.693868142014267));
#28810=CARTESIAN_POINT('Ctrl Pts',(-12.0246518208346,-0.433398242012175,
-1.94716905024808));
#28811=CARTESIAN_POINT('Ctrl Pts',(-11.9136303237558,1.39939082021156,-1.42162114458219));
#28812=CARTESIAN_POINT('Ctrl Pts',(-11.802608826677,1.9537573949821,0.402657904391348));
#28813=CARTESIAN_POINT('Ctrl Pts',(-11.6915873295982,0.723256331137679,
1.85908623411803));
#28814=CARTESIAN_POINT('Ctrl Pts',(-11.5805658325193,-1.16798020743223,
1.61713437334789));
#28815=CARTESIAN_POINT('Ctrl Pts',(-11.4695443354405,-1.99220091274483,
-0.102160998798728));
#28816=CARTESIAN_POINT('Ctrl Pts',(-11.3585228383617,-0.996433656445175,
-1.72812653319149));
#28817=CARTESIAN_POINT('Ctrl Pts',(-11.2475013412829,0.909631977730951,
-1.77535095446118));
#28818=CARTESIAN_POINT('Ctrl Pts',(-11.136479844204,1.98469746609999,-0.200692088716223));
#28819=CARTESIAN_POINT('Ctrl Pts',(-11.0254583471252,1.24662981481611,1.5573103259237));
#28820=CARTESIAN_POINT('Ctrl Pts',(-10.9144368500464,-0.630304524580239,
1.89262187261763));
#28821=CARTESIAN_POINT('Ctrl Pts',(-10.8034153529676,-1.93142011018166,
0.498916530496676));
#28822=CARTESIAN_POINT('Ctrl Pts',(-10.6923938558887,-1.46807442741462,
-1.35057721807686));
#28823=CARTESIAN_POINT('Ctrl Pts',(-10.5813723588099,0.336440094073728,
-1.96624245949391));
#28824=CARTESIAN_POINT('Ctrl Pts',(-10.4703508617311,1.83359760297329,-0.785634251282103));
#28825=CARTESIAN_POINT('Ctrl Pts',(-10.3593293646522,1.65566022435232,1.11269518194096));
#28826=CARTESIAN_POINT('Ctrl Pts',(-10.2483078675734,-0.0348162047050451,
1.99451477264695));
#28827=CARTESIAN_POINT('Ctrl Pts',(-10.1372863704946,-1.69348606594746,
1.05423256013973));
#28828=CARTESIAN_POINT('Ctrl Pts',(-10.0262648734158,-1.80506083579367,
-0.849150590590889));
#28829=CARTESIAN_POINT('Ctrl Pts',(-9.91524337633695,-0.267610665381181,
-1.97678675587207));
#28830=CARTESIAN_POINT('Ctrl Pts',(-9.80422187925813,1.51431695019108,-1.29851666172637));
#28831=CARTESIAN_POINT('Ctrl Pts',(-9.69320038217929,1.91283057283628,0.56602168336543));
#28832=CARTESIAN_POINT('Ctrl Pts',(-9.58217888510047,0.563865518559531,
1.9134672778484));
#28833=CARTESIAN_POINT('Ctrl Pts',(-9.47115738802165,-1.30022250809489,
1.51285252944907));
#28834=CARTESIAN_POINT('Ctrl Pts',(-9.36013589094282,-1.97648389687789,
-0.269838380886415));
#28835=CARTESIAN_POINT('Ctrl Pts',(-9.24911439386399,-0.847115705016716,
-1.80601670222925));
#28836=CARTESIAN_POINT('Ctrl Pts',(-9.13809289678518,1.05614048948519,-1.69229684538114));
#28837=CARTESIAN_POINT('Ctrl Pts',(-9.02707139970634,1.99455274463459,-0.0325683172365964));
#28838=CARTESIAN_POINT('Ctrl Pts',(-8.91604990262752,1.11082850701714,1.65691320666324));
#28839=CARTESIAN_POINT('Ctrl Pts',(-8.80502840554869,-0.787700260230558,
1.83271101007488));
#28840=CARTESIAN_POINT('Ctrl Pts',(-8.69400690846987,-1.96662038669951,
0.334223878612652));
#28841=CARTESIAN_POINT('Ctrl Pts',(-8.58298541139104,-1.34892180570934,
-1.46959562754482));
#28842=CARTESIAN_POINT('Ctrl Pts',(-8.47196391431221,0.501092969818087,
-1.93085659281467));
#28843=CARTESIAN_POINT('Ctrl Pts',(-8.3609424172334,1.8933310387477,-0.62817109463232));
#28844=CARTESIAN_POINT('Ctrl Pts',(-8.24992092015456,1.55590435558153,1.24838414868958));
#28845=CARTESIAN_POINT('Ctrl Pts',(-8.13889942307575,-0.20292876227853,
1.98447002090158));
#28846=CARTESIAN_POINT('Ctrl Pts',(-8.0278779259969,-1.77637500372011,0.907630537485031));
#28847=CARTESIAN_POINT('Ctrl Pts',(-7.9168564289181,-1.72700243135777,-0.998380663124713));
#28848=CARTESIAN_POINT('Ctrl Pts',(-7.80583493183926,-0.0999156763351079,
-1.99231478537893));
#28849=CARTESIAN_POINT('Ctrl Pts',(-7.69481343476044,1.61844968765863,-1.16615691694329));
#28850=CARTESIAN_POINT('Ctrl Pts',(-7.58379193768161,1.85826992642422,0.725351105992336));
#28851=CARTESIAN_POINT('Ctrl Pts',(-7.47277044060279,0.400455717839537,
1.95420995915655));
#28852=CARTESIAN_POINT('Ctrl Pts',(-7.36174894352396,-1.42319738830023,
1.39778773079191));
#28853=CARTESIAN_POINT('Ctrl Pts',(-7.25072744644514,-1.94667936353946,
-0.435592472371381));
#28854=CARTESIAN_POINT('Ctrl Pts',(-7.13970594936631,-0.691759881327519,
-1.87103436980797));
#28855=CARTESIAN_POINT('Ctrl Pts',(-7.02868445228748,1.19512129123814,-1.59718078051493));
#28856=CARTESIAN_POINT('Ctrl Pts',(-6.91766295520866,1.99019171881064,0.135787587041479));
#28857=CARTESIAN_POINT('Ctrl Pts',(-6.80664145812983,0.967109696816501,
1.74470633080198));
#28858=CARTESIAN_POINT('Ctrl Pts',(-6.69561996105101,-0.939481611065625,
1.75973738065841));
#28859=CARTESIAN_POINT('Ctrl Pts',(-6.58459846397218,-1.98780344855593,
0.16714902430503));
#28860=CARTESIAN_POINT('Ctrl Pts',(-6.47357696689336,-1.22015465613688,
-1.57813939863514));
#28861=CARTESIAN_POINT('Ctrl Pts',(-6.36255546981452,0.662174272842673,
-1.88170842024004));
#28862=CARTESIAN_POINT('Ctrl Pts',(-6.25153397273571,1.93956963445295,-0.466230607666484));
#28863=CARTESIAN_POINT('Ctrl Pts',(-6.14051247565688,1.44505867736286,1.37517517625766));
#28864=CARTESIAN_POINT('Ctrl Pts',(-6.02949097857805,-0.369594931905942,
1.96028083006656));
#28865=CARTESIAN_POINT('Ctrl Pts',(-5.91846948149923,-1.84660271316689,
0.754559319166941));
#28866=CARTESIAN_POINT('Ctrl Pts',(-5.8074479844204,-1.63663470481537,-1.14049471257472));
#28867=CARTESIAN_POINT('Ctrl Pts',(-5.69642648734157,0.0684914681898172,
-1.99364246172733));
#28868=CARTESIAN_POINT('Ctrl Pts',(-5.58540499026275,1.71104681975768,-1.02548531291975));
#28869=CARTESIAN_POINT('Ctrl Pts',(-5.47438349318392,1.79046434030052,0.879510541454284));
#28870=CARTESIAN_POINT('Ctrl Pts',(-5.3633619961051,0.234191642955949,1.98102388193242));
#28871=CARTESIAN_POINT('Ctrl Pts',(-5.25234049902627,-1.53602833659461,
1.27276010920966));
#28872=CARTESIAN_POINT('Ctrl Pts',(-5.14131900194745,-1.90299974647861,
-0.598241850190491));
#28873=CARTESIAN_POINT('Ctrl Pts',(-5.03029750486863,-0.531473494111017,
-1.92271611827498));
#28874=CARTESIAN_POINT('Ctrl Pts',(-4.91927600778979,1.32558378828978,-1.49068070579863));
#28875=CARTESIAN_POINT('Ctrl Pts',(-4.80825451071098,1.97164547212322,0.303175656465004));
#28876=CARTESIAN_POINT('Ctrl Pts',(-4.69723301363214,0.816497749377447,
1.82006394713993));
#28877=CARTESIAN_POINT('Ctrl Pts',(-4.58621151655333,-1.08456674563962,
1.6742211086561));
#28878=CARTESIAN_POINT('Ctrl Pts',(-4.47519001947449,-1.99481831210039,
-0.0011171955401132));
#28879=CARTESIAN_POINT('Ctrl Pts',(-4.36416852239567,-1.08269077492733,
-1.67543487856269));
#28880=CARTESIAN_POINT('Ctrl Pts',(-4.25314702531684,0.818535885687912,
-1.81914824856525));
#28881=CARTESIAN_POINT('Ctrl Pts',(-4.14212552823802,1.97198382149198,-0.300967031733712));
#28882=CARTESIAN_POINT('Ctrl Pts',(-4.03110403115918,1.32391324947435,1.49216455335334));
#28883=CARTESIAN_POINT('Ctrl Pts',(-3.92008253408037,-0.533626789628149,
1.92211961017187));
#28884=CARTESIAN_POINT('Ctrl Pts',(-3.80906103700153,-1.90366864172245,
0.596109930246183));
#28885=CARTESIAN_POINT('Ctrl Pts',(-3.69803953992272,-1.53460175801352,
-1.27447981181542));
#28886=CARTESIAN_POINT('Ctrl Pts',(-3.58701804284388,0.236410435324478,
-1.9807603218156));
#28887=CARTESIAN_POINT('Ctrl Pts',(-3.47599654576507,1.79144835440527,-0.877504495662993));
#28888=CARTESIAN_POINT('Ctrl Pts',(-3.36497504868623,1.70989710319601,1.02740120836059));
#28889=CARTESIAN_POINT('Ctrl Pts',(-3.25395355160742,0.0662583518974708,
1.99371792818321));
#28890=CARTESIAN_POINT('Ctrl Pts',(-3.14293205452858,-1.63791114303142,
1.13866080723203));
#28891=CARTESIAN_POINT('Ctrl Pts',(-3.03191055744976,-1.84575637505747,
-0.756627220383344));
#28892=CARTESIAN_POINT('Ctrl Pts',(-2.92088906037093,-0.36739899491419,
-1.96069358250483));
#28893=CARTESIAN_POINT('Ctrl Pts',(-2.80986756329211,1.44659810052314,-1.37355570763518));
#28894=CARTESIAN_POINT('Ctrl Pts',(-2.69884606621328,1.9390461945082,0.468402822060808));
#28895=CARTESIAN_POINT('Ctrl Pts',(-2.58782456913446,0.660066160467937,
1.88244893865578));
#28896=CARTESIAN_POINT('Ctrl Pts',(-2.47680307205563,-1.22192155893126,
1.57677171821057));
#28897=CARTESIAN_POINT('Ctrl Pts',(-2.36578157497681,-1.98761498089598,
-0.169375455078507));
#28898=CARTESIAN_POINT('Ctrl Pts',(-2.25476007789798,-0.937509940151467,
-1.76078858256476));
#28899=CARTESIAN_POINT('Ctrl Pts',(-2.14373858081916,0.969063321888055,
-1.74362198881325));
#28900=CARTESIAN_POINT('Ctrl Pts',(-2.03271708374032,1.99034258258444,-0.133558275957203));
#28901=CARTESIAN_POINT('Ctrl Pts',(-1.92169558666151,1.19333151158385,1.59851839679231));
#28902=CARTESIAN_POINT('Ctrl Pts',(-1.81067408958268,-0.693855126354071,
1.87025842209972));
#28903=CARTESIAN_POINT('Ctrl Pts',(-1.69965259250386,-1.94716616503712,
0.433411606672418));
#28904=CARTESIAN_POINT('Ctrl Pts',(-1.58863109542502,-1.42163061521549,
-1.39938074047672));
#28905=CARTESIAN_POINT('Ctrl Pts',(-1.4776095983462,0.402643948884029,-1.95376062705992));
#28906=CARTESIAN_POINT('Ctrl Pts',(-1.36658810126737,1.85908202905433,-0.723268364827023));
#28907=CARTESIAN_POINT('Ctrl Pts',(-1.25556660418855,1.61714093219328,1.16796740173245));
#28908=CARTESIAN_POINT('Ctrl Pts',(-1.14454510710972,-0.102144286227503,
1.9922046737893));
#28909=CARTESIAN_POINT('Ctrl Pts',(-1.0335236100309,-1.72812517579298,0.99643981569525));
#28910=CARTESIAN_POINT('Ctrl Pts',(-0.922502112952074,-1.77534670427177,
-0.909608623609972));
#28911=CARTESIAN_POINT('Ctrl Pts',(-0.811480615873249,-0.200725913054806,
-1.98471711706149));
#28912=CARTESIAN_POINT('Ctrl Pts',(-0.700459118794423,1.55733989746973,
-1.24660056130178));
#28913=CARTESIAN_POINT('Ctrl Pts',(-0.589437621715598,1.89255353070104,
0.630215218936021));
#28914=CARTESIAN_POINT('Ctrl Pts',(-0.478416124636772,0.499068295829763,
1.93156167278018));
#28915=CARTESIAN_POINT('Ctrl Pts',(-0.367394627557947,-1.3508306443166,
1.4678076366454));
#28916=CARTESIAN_POINT('Ctrl Pts',(-0.25637313047912,-1.96574101035108,
-0.335899396150099));
#28917=CARTESIAN_POINT('Ctrl Pts',(-0.145351633400296,-0.78662434608425,
-1.83460887189422));
#28918=CARTESIAN_POINT('Ctrl Pts',(-0.0343301363214683,1.11470387286102,
-1.65361507057469));
#28919=CARTESIAN_POINT('Ctrl Pts',(0.0396841950644149,1.69786070835726,
-0.531282356819573));
#28920=CARTESIAN_POINT('Ctrl Pts',(0.0766913607573572,1.68807636917386,
0.0294553268735078));
#28921=CARTESIAN_POINT('Ctrl Pts',(-15.7226913607574,-0.802959149489957,
1.63459616787393));
#28922=CARTESIAN_POINT('Ctrl Pts',(-15.6856841950644,-1.34593201830381,
1.36787277679565));
#28923=CARTESIAN_POINT('Ctrl Pts',(-15.6116698636785,-2.13591160079902,
0.255552036473978));
#28924=CARTESIAN_POINT('Ctrl Pts',(-15.5006483665997,-1.37338031410794,
-1.65832692067852));
#28925=CARTESIAN_POINT('Ctrl Pts',(-15.3896268695209,0.645581844690631,
-2.05197493134485));
#28926=CARTESIAN_POINT('Ctrl Pts',(-15.278605372442,2.07385877578268,-0.573662929393826));
#28927=CARTESIAN_POINT('Ctrl Pts',(-15.1675838753632,1.60802441494309,1.43009236470613));
#28928=CARTESIAN_POINT('Ctrl Pts',(-15.0565623782844,-0.327080723815373,
2.12665944556502));
#28929=CARTESIAN_POINT('Ctrl Pts',(-14.9455408812056,-1.96324796184311,
0.880780288573345));
#28930=CARTESIAN_POINT('Ctrl Pts',(-14.8345193841267,-1.80594633577617,
-1.1699395550268));
#28931=CARTESIAN_POINT('Ctrl Pts',(-14.7234978870479,0.00122541408525625,
-2.15174944545788));
#28932=CARTESIAN_POINT('Ctrl Pts',(-14.6124763899691,1.8072586404345,-1.1678695140996));
#28933=CARTESIAN_POINT('Ctrl Pts',(-14.5014548928903,1.9622691127951,0.882953885847407));
#28934=CARTESIAN_POINT('Ctrl Pts',(-14.3904333958115,0.32463075438992,2.1271339690297));
#28935=CARTESIAN_POINT('Ctrl Pts',(-14.2794118987326,-1.60957335547925,
1.42806507104192));
#28936=CARTESIAN_POINT('Ctrl Pts',(-14.1683904016538,-2.07334282239369,
-0.575626034370439));
#28937=CARTESIAN_POINT('Ctrl Pts',(-14.057368904575,-0.642995851091954,
-2.05344807925839));
#28938=CARTESIAN_POINT('Ctrl Pts',(-13.9463474074961,1.37476371604704,-1.65533057206896));
#28939=CARTESIAN_POINT('Ctrl Pts',(-13.8353259104173,2.13659925589318,0.255025435270031));
#28940=CARTESIAN_POINT('Ctrl Pts',(-13.7243044133385,0.946530687964835,
1.93240099710466));
#28941=CARTESIAN_POINT('Ctrl Pts',(-13.6132829162597,-1.10824702172465,
1.84441936227157));
#28942=CARTESIAN_POINT('Ctrl Pts',(-13.5022614191808,-2.15057856485875,
0.0714564641882035));
#28943=CARTESIAN_POINT('Ctrl Pts',(-13.391239922102,-1.22823520722557,-1.76678590031394));
#28944=CARTESIAN_POINT('Ctrl Pts',(-13.2802184250232,0.816170317961378,
-1.99096966239773));
#28945=CARTESIAN_POINT('Ctrl Pts',(-13.1691969279444,2.11495820239117,-0.396290266790191));
#28946=CARTESIAN_POINT('Ctrl Pts',(-13.0581754308655,1.48161241110288,1.56042264506286));
#28947=CARTESIAN_POINT('Ctrl Pts',(-12.9471539337867,-0.505269929782832,
2.09160141331823));
#28948=CARTESIAN_POINT('Ctrl Pts',(-12.8361324367079,-2.03055967606441,
0.711984251270878));
#28949=CARTESIAN_POINT('Ctrl Pts',(-12.7251109396291,-1.70081856536528,
-1.31807070344234));
#28950=CARTESIAN_POINT('Ctrl Pts',(-12.6140894425502,0.182716288572517,
-2.14399368710076));
#28951=CARTESIAN_POINT('Ctrl Pts',(-12.5030679454714,1.899329501586,-1.01125744323421));
#28952=CARTESIAN_POINT('Ctrl Pts',(-12.3920464483926,1.88079802813469,1.04531954416464));
#28953=CARTESIAN_POINT('Ctrl Pts',(-12.2810249513138,0.144051415096028,
2.14693813650445));
#28954=CARTESIAN_POINT('Ctrl Pts',(-12.1700034542349,-1.72429429504063,
1.28720758085167));
#28955=CARTESIAN_POINT('Ctrl Pts',(-12.0589819571561,-2.01739985786644,
-0.748459742131278));
#28956=CARTESIAN_POINT('Ctrl Pts',(-11.9479604600773,-0.467496800638412,
-2.10036685212841));
#28957=CARTESIAN_POINT('Ctrl Pts',(-11.8369389629985,1.50949096667834,-1.53347031064656));
#28958=CARTESIAN_POINT('Ctrl Pts',(-11.7259174659196,2.10747354935533,0.434337899435756));
#28959=CARTESIAN_POINT('Ctrl Pts',(-11.6148959688408,0.780160111583563,
2.00535392697016));
#28960=CARTESIAN_POINT('Ctrl Pts',(-11.503874471762,-1.25987361565765,1.74436597211969));
#28961=CARTESIAN_POINT('Ctrl Pts',(-11.3928529746832,-2.14894169531716,
-0.110198739770348));
#28962=CARTESIAN_POINT('Ctrl Pts',(-11.2818314776043,-1.07483026297892,
-1.86409068392728));
#28963=CARTESIAN_POINT('Ctrl Pts',(-11.1708099805255,0.981199271536627,
-1.91503059026627));
#28964=CARTESIAN_POINT('Ctrl Pts',(-11.0597884834467,2.14084789852661,-0.216481979605357));
#28965=CARTESIAN_POINT('Ctrl Pts',(-10.9487669863679,1.34471115365209,1.67983513636409));
#28966=CARTESIAN_POINT('Ctrl Pts',(-10.837745489289,-0.679895117481559,
2.04152805548794));
#28967=CARTESIAN_POINT('Ctrl Pts',(-10.7267239922102,-2.08337882961056,
0.538169884376828));
#28968=CARTESIAN_POINT('Ctrl Pts',(-10.6157024951314,-1.58357840753797,
-1.45683684717925));
#28969=CARTESIAN_POINT('Ctrl Pts',(-10.5046809980526,0.362910257447538,
-2.12094090374037));
#28970=CARTESIAN_POINT('Ctrl Pts',(-10.3936595009737,1.9778599217857,-0.847445751605094));
#28971=CARTESIAN_POINT('Ctrl Pts',(-10.2826380038949,1.78592292907185,1.20023891935526));
#28972=CARTESIAN_POINT('Ctrl Pts',(-10.1716165068161,-0.0375554460821274,
2.15143760322934));
#28973=CARTESIAN_POINT('Ctrl Pts',(-10.0605950097372,-1.82672480183691,
1.13717662237383));
#28974=CARTESIAN_POINT('Ctrl Pts',(-9.94957351265842,-1.94707796176875,
-0.915959378419207));
#28975=CARTESIAN_POINT('Ctrl Pts',(-9.83855201557959,-0.288665522272483,
-2.13231479579607));
#28976=CARTESIAN_POINT('Ctrl Pts',(-9.72753051850077,1.63345916236307,-1.40068031220968));
#28977=CARTESIAN_POINT('Ctrl Pts',(-9.61650902142194,2.06332671958362,0.610554682540373));
#28978=CARTESIAN_POINT('Ctrl Pts',(-9.50548752434312,0.608228876732484,
2.06401351876105));
#28979=CARTESIAN_POINT('Ctrl Pts',(-9.39446602726429,-1.40252036978803,
1.63187952510266));
#28980=CARTESIAN_POINT('Ctrl Pts',(-9.28344453018547,-2.1319881087053,-0.291068508188133));
#28981=CARTESIAN_POINT('Ctrl Pts',(-9.17242303310663,-0.913764393752982,
-1.94810903309566));
#28982=CARTESIAN_POINT('Ctrl Pts',(-9.06140153602782,1.1392346622512,-1.82544201673049));
#28983=CARTESIAN_POINT('Ctrl Pts',(-8.95038003894899,2.15147856274651,-0.0351307011297477));
#28984=CARTESIAN_POINT('Ctrl Pts',(-8.83935854187017,1.19822537968178,1.78727449251818));
#28985=CARTESIAN_POINT('Ctrl Pts',(-8.72833704479134,-0.849674308345434,
1.97690357424366));
#28986=CARTESIAN_POINT('Ctrl Pts',(-8.61731554771251,-2.12134856519896,
0.360519676367277));
#28987=CARTESIAN_POINT('Ctrl Pts',(-8.5062940506337,-1.4550511916077,-1.58521929142964));
#28988=CARTESIAN_POINT('Ctrl Pts',(-8.39527255355485,0.540517559842268,
-2.08277097627699));
#28989=CARTESIAN_POINT('Ctrl Pts',(-8.28425105647605,2.04229301682093,-0.677593835246537));
#28990=CARTESIAN_POINT('Ctrl Pts',(-8.1732295593972,1.67831854821712,1.34660351359635));
#28991=CARTESIAN_POINT('Ctrl Pts',(-8.06220806231839,-0.218894628372896,
2.14060255857764));
#28992=CARTESIAN_POINT('Ctrl Pts',(-7.95118656523956,-1.91613520884992,
0.979040363583317));
#28993=CARTESIAN_POINT('Ctrl Pts',(-7.84016506816073,-1.86287814091277,
-1.07693045468546));
#28994=CARTESIAN_POINT('Ctrl Pts',(-7.7291435710819,-0.107776761630186,
-2.14906452713085));
#28995=CARTESIAN_POINT('Ctrl Pts',(-7.61812207400309,1.74578477167283,-1.25790687378474));
#28996=CARTESIAN_POINT('Ctrl Pts',(-7.50710057692426,2.00447339447557,0.78241969745096));
#28997=CARTESIAN_POINT('Ctrl Pts',(-7.39607907984543,0.431962451020007,
2.10796172001022));
#28998=CARTESIAN_POINT('Ctrl Pts',(-7.2850575827666,-1.53517056880124,1.50776175067752));
#28999=CARTESIAN_POINT('Ctrl Pts',(-7.17403608568778,-2.09983863824241,
-0.469863666890626));
#29000=CARTESIAN_POINT('Ctrl Pts',(-7.06301458860895,-0.74618560940433,
-2.01824210847894));
#29001=CARTESIAN_POINT('Ctrl Pts',(-6.95199309153013,1.28915008384591,-1.7228424865436));
#29002=CARTESIAN_POINT('Ctrl Pts',(-6.8409715944513,2.1467744236371,0.146470973702092));
#29003=CARTESIAN_POINT('Ctrl Pts',(-6.72995009737248,1.04319917641796,1.88197493353141));
#29004=CARTESIAN_POINT('Ctrl Pts',(-6.61892860029365,-1.01339739033702,
1.8981885842502));
#29005=CARTESIAN_POINT('Ctrl Pts',(-6.50790710321483,-2.1441982509744,0.180299840926073));
#29006=CARTESIAN_POINT('Ctrl Pts',(-6.396885606136,-1.31615300371251,-1.70230298212104));
#29007=CARTESIAN_POINT('Ctrl Pts',(-6.28586410905717,0.714272288188727,
-2.02975596327374));
#29008=CARTESIAN_POINT('Ctrl Pts',(-6.17484261197835,2.09216953560388,-0.502912324775098));
#29009=CARTESIAN_POINT('Ctrl Pts',(-6.06382111489953,1.55875184279803,1.48337010374802));
#29010=CARTESIAN_POINT('Ctrl Pts',(-5.95279961782069,-0.398673624969019,
2.11451023002342));
#29011=CARTESIAN_POINT('Ctrl Pts',(-5.84177812074189,-1.9918882375888,0.813925930951356));
#29012=CARTESIAN_POINT('Ctrl Pts',(-5.73075662366303,-1.7654005349968,-1.23022563912181));
#29013=CARTESIAN_POINT('Ctrl Pts',(-5.61973512658423,0.0738801848874695,
-2.15049666133214));
#29014=CARTESIAN_POINT('Ctrl Pts',(-5.50871362950539,1.8456671865244,-1.10616762233703));
#29015=CARTESIAN_POINT('Ctrl Pts',(-5.39769213242658,1.93133305493226,0.948707965100779));
#29016=CARTESIAN_POINT('Ctrl Pts',(-5.28667063534773,0.252617184854861,
2.13688528705583));
#29017=CARTESIAN_POINT('Ctrl Pts',(-5.17564913826893,-1.65687873977979,
1.37289730635085));
#29018=CARTESIAN_POINT('Ctrl Pts',(-5.06462764119009,-2.05272243136938,
-0.645309841760259));
#29019=CARTESIAN_POINT('Ctrl Pts',(-4.95360614411127,-0.573288338613145,
-2.07399003202278));
#29020=CARTESIAN_POINT('Ctrl Pts',(-4.84258464703244,1.42987700440694,-1.60796328452731));
#29021=CARTESIAN_POINT('Ctrl Pts',(-4.73156314995361,2.12676901025572,0.327028667146397));
#29022=CARTESIAN_POINT('Ctrl Pts',(-4.62054165287479,0.880737503203102,
1.9632614758537));
#29023=CARTESIAN_POINT('Ctrl Pts',(-4.50952015579596,-1.16989741654532,
1.80594413171622));
#29024=CARTESIAN_POINT('Ctrl Pts',(-4.39849865871714,-2.151765024316,-0.00120509335308468));
#29025=CARTESIAN_POINT('Ctrl Pts',(-4.28747716163831,-1.16787384971678,
-1.80725339763617));
#29026=CARTESIAN_POINT('Ctrl Pts',(-4.17645566455949,0.882935994364434,
-1.96227373268238));
#29027=CARTESIAN_POINT('Ctrl Pts',(-4.06543416748067,2.12713398000424,-0.324646274013261));
#29028=CARTESIAN_POINT('Ctrl Pts',(-3.95441267040183,1.42807503228097,1.60956387704757));
#29029=CARTESIAN_POINT('Ctrl Pts',(-3.84339117332301,-0.575611049384669,
2.07334659233446));
#29030=CARTESIAN_POINT('Ctrl Pts',(-3.73236967624418,-2.05344395341572,
0.643010188331699));
#29031=CARTESIAN_POINT('Ctrl Pts',(-3.62134817916536,-1.65533992199544,
-1.37475231033633));
#29032=CARTESIAN_POINT('Ctrl Pts',(-3.51032668208653,0.255010545586425,
-2.13660099076793));
#29033=CARTESIAN_POINT('Ctrl Pts',(-3.39930518500771,1.93239448850803,-0.946544089250699));
#29034=CARTESIAN_POINT('Ctrl Pts',(-3.28828368792888,1.84442701348695,1.10823425505983));
#29035=CARTESIAN_POINT('Ctrl Pts',(-3.17726219085005,0.0714713732659194,
2.15057806527719));
#29036=CARTESIAN_POINT('Ctrl Pts',(-3.06624069377123,-1.76677739979312,
1.22824744724822));
#29037=CARTESIAN_POINT('Ctrl Pts',(-2.9552191966924,-1.99097531196969,-0.81615652883798));
#29038=CARTESIAN_POINT('Ctrl Pts',(-2.84419769961358,-0.396304917811199,
-2.11495545666636));
#29039=CARTESIAN_POINT('Ctrl Pts',(-2.73317620253476,1.56041238345669,-1.4816232198746));
#29040=CARTESIAN_POINT('Ctrl Pts',(-2.62215470545592,2.09160491287177,0.505255442908033));
#29041=CARTESIAN_POINT('Ctrl Pts',(-2.5111332083771,0.711998315442568,2.03055474360234));
#29042=CARTESIAN_POINT('Ctrl Pts',(-2.40011171129828,-1.31805892146514,
1.70082769643504));
#29043=CARTESIAN_POINT('Ctrl Pts',(-2.28909021421945,-2.14399495520735,
-0.182701441030875));
#29044=CARTESIAN_POINT('Ctrl Pts',(-2.17806871714062,-1.01127059388303,
-1.89932249177543));
#29045=CARTESIAN_POINT('Ctrl Pts',(-2.0670472200618,1.04530650723304,-1.88080527855502));
#29046=CARTESIAN_POINT('Ctrl Pts',(-1.95602572298297,2.14693715694967,-0.144066266671712));
#29047=CARTESIAN_POINT('Ctrl Pts',(-1.84500422590415,1.28721948934618,1.72428534271959));
#29048=CARTESIAN_POINT('Ctrl Pts',(-1.73398272882532,-0.748445702435426,
2.01740511138042));
#29049=CARTESIAN_POINT('Ctrl Pts',(-1.6229612317465,-2.10036373991713,0.467511216792655));
#29050=CARTESIAN_POINT('Ctrl Pts',(-1.51193973466767,-1.53348052640274,
-1.50948009389823));
#29051=CARTESIAN_POINT('Ctrl Pts',(-1.40091823758885,0.434322845948246,
-2.10747703572397));
#29052=CARTESIAN_POINT('Ctrl Pts',(-1.28989674051002,2.00534939106384,-0.780173092049846));
#29053=CARTESIAN_POINT('Ctrl Pts',(-1.1788752434312,1.74437304699665,1.25985980244131));
#29054=CARTESIAN_POINT('Ctrl Pts',(-1.06785374635237,-0.110180712300874,
2.14894575227006));
#29055=CARTESIAN_POINT('Ctrl Pts',(-0.956832249273545,-1.86408921973246,
1.07483690682153));
#29056=CARTESIAN_POINT('Ctrl Pts',(-0.845810752194719,-1.91502600568388,
-0.981174079978886));
#29057=CARTESIAN_POINT('Ctrl Pts',(-0.734789255115894,-0.216518465148069,
-2.14086909557066));
#29058=CARTESIAN_POINT('Ctrl Pts',(-0.623767758037068,1.67986703451646,
-1.34467959855327));
#29059=CARTESIAN_POINT('Ctrl Pts',(-0.512746260958242,2.04145433662096,
0.67979878551963));
#29060=CARTESIAN_POINT('Ctrl Pts',(-0.401724763879417,0.538333590180839,
2.08353152995745));
#29061=CARTESIAN_POINT('Ctrl Pts',(-0.290703266800591,-1.45711021228504,
1.58329062641899));
#29062=CARTESIAN_POINT('Ctrl Pts',(-0.179681769721765,-2.12040000198483,
-0.362327018927154));
#29063=CARTESIAN_POINT('Ctrl Pts',(-0.0686602726429408,-0.84851374429049,
-1.97895075451018));
#29064=CARTESIAN_POINT('Ctrl Pts',(0.0423612244358866,1.20240564844544,
-1.78371686832869));
#29065=CARTESIAN_POINT('Ctrl Pts',(0.11637555582177,1.83144362884697,-0.573082163175473));
#29066=CARTESIAN_POINT('Ctrl Pts',(0.153382721514712,1.82088948528754,0.0317727894123157));
#29067=CARTESIAN_POINT('Ctrl Pts',(-15.646,-0.861525859670559,1.75382131162753));
#29068=CARTESIAN_POINT('Ctrl Pts',(-15.6089928343071,-1.44410240528908,
1.46764349182322));
#29069=CARTESIAN_POINT('Ctrl Pts',(-15.5349785029212,-2.29170198661735,
0.274191642319117));
#29070=CARTESIAN_POINT('Ctrl Pts',(-15.4239570058423,-1.47355274115507,
-1.7792829521401));
#29071=CARTESIAN_POINT('Ctrl Pts',(-15.3129355087636,0.692669675771291,
-2.20164309463595));
#29072=CARTESIAN_POINT('Ctrl Pts',(-15.2019140116847,2.22512311588507,-0.615505096020252));
#29073=CARTESIAN_POINT('Ctrl Pts',(-15.0908925146059,1.72531145243826,1.53440128890039));
#29074=CARTESIAN_POINT('Ctrl Pts',(-14.979871017527,-0.350937531436932,
2.28177499220319));
#29075=CARTESIAN_POINT('Ctrl Pts',(-14.8688495204482,-2.10644450486397,
0.945023163103684));
#29076=CARTESIAN_POINT('Ctrl Pts',(-14.7578280233694,-1.93766951959731,
-1.25527329945402));
#29077=CARTESIAN_POINT('Ctrl Pts',(-14.6468065262906,0.00131479406382864,
-2.3086950213735));
#29078=CARTESIAN_POINT('Ctrl Pts',(-14.5357850292118,1.93907754191032,-1.25305227265524));
#29079=CARTESIAN_POINT('Ctrl Pts',(-14.4247635321329,2.10539425994415,0.947355299503518));
#29080=CARTESIAN_POINT('Ctrl Pts',(-14.3137420350541,0.348308864689988,
2.28228412674149));
#29081=CARTESIAN_POINT('Ctrl Pts',(-14.2027205379753,-1.72697337051695,
1.53222612728979));
#29082=CARTESIAN_POINT('Ctrl Pts',(-14.0916990408964,-2.22456952958211,
-0.617611387110731));
#29083=CARTESIAN_POINT('Ctrl Pts',(-13.9806775438176,-0.689895063439384,
-2.20322369188481));
#29084=CARTESIAN_POINT('Ctrl Pts',(-13.8696560467388,1.47503704648443,-1.7760680540804));
#29085=CARTESIAN_POINT('Ctrl Pts',(-13.75863454966,2.29243979830618,0.273626631564544));
#29086=CARTESIAN_POINT('Ctrl Pts',(-13.6476130525811,1.01556930408161,2.0733476059353));
#29087=CARTESIAN_POINT('Ctrl Pts',(-13.5365915555023,-1.18908099960645,
1.97894871449363));
#29088=CARTESIAN_POINT('Ctrl Pts',(-13.4255700584235,-2.30743873839151,
0.0766683981095072));
#29089=CARTESIAN_POINT('Ctrl Pts',(-13.3145485613447,-1.31782095447173,
-1.89565277709167));
#29090=CARTESIAN_POINT('Ctrl Pts',(-13.2035270642658,0.875700632175267,
-2.13618818723813));
#29091=CARTESIAN_POINT('Ctrl Pts',(-13.092505567187,2.26922027682201,-0.425195121062348));
#29092=CARTESIAN_POINT('Ctrl Pts',(-12.9814840701082,1.5896791349657,1.67423767646352));
#29093=CARTESIAN_POINT('Ctrl Pts',(-12.8704625730294,-0.542123607282315,
2.24415987642929));
#29094=CARTESIAN_POINT('Ctrl Pts',(-12.7594410759505,-2.17866584077781,
0.763915380424621));
#29095=CARTESIAN_POINT('Ctrl Pts',(-12.6484195788717,-1.82487387758237,
-1.41420892533704));
#29096=CARTESIAN_POINT('Ctrl Pts',(-12.5373980817929,0.196043357483676,
-2.30037356891822));
#29097=CARTESIAN_POINT('Ctrl Pts',(-12.426376584714,2.03786392208238,-1.08501713777596));
#29098=CARTESIAN_POINT('Ctrl Pts',(-12.3153550876352,2.01798078904102,1.12156368040506));
#29099=CARTESIAN_POINT('Ctrl Pts',(-12.2043335905564,0.154558322557508,
2.30353278231703));
#29100=CARTESIAN_POINT('Ctrl Pts',(-12.0933120934776,-1.85006189393761,
1.38109469002517));
#29101=CARTESIAN_POINT('Ctrl Pts',(-11.9822905963987,-2.16454616396323,
-0.803051342248286));
#29102=CARTESIAN_POINT('Ctrl Pts',(-11.8712690993199,-0.501595359264648,
-2.25356465400873));
#29103=CARTESIAN_POINT('Ctrl Pts',(-11.7602476022411,1.61959111314513,-1.64531947671092));
#29104=CARTESIAN_POINT('Ctrl Pts',(-11.6492261051623,2.26118970372855,0.466017894480162));
#29105=CARTESIAN_POINT('Ctrl Pts',(-11.5382046080835,0.837063892029446,
2.15162161982229));
#29106=CARTESIAN_POINT('Ctrl Pts',(-11.4271831110046,-1.35176702388306,
1.87159757089149));
#29107=CARTESIAN_POINT('Ctrl Pts',(-11.3161616139258,-2.30568247788948,
-0.118236480741969));
#29108=CARTESIAN_POINT('Ctrl Pts',(-11.205140116847,-1.15322686951267,-2.00005483466307));
#29109=CARTESIAN_POINT('Ctrl Pts',(-11.0941186197681,1.05276656534231,-2.05471022607136));
#29110=CARTESIAN_POINT('Ctrl Pts',(-10.9830971226893,2.29699833095323,-0.232271870494488));
#29111=CARTESIAN_POINT('Ctrl Pts',(-10.8720756256105,1.44279249248807,1.80235994680447));
#29112=CARTESIAN_POINT('Ctrl Pts',(-10.7610541285317,-0.729485710382879,
2.19043423835826));
#29113=CARTESIAN_POINT('Ctrl Pts',(-10.6500326314528,-2.23533754903947,
0.577423238256977));
#29114=CARTESIAN_POINT('Ctrl Pts',(-10.539011134374,-1.69908238766131,-1.56309647628163));
#29115=CARTESIAN_POINT('Ctrl Pts',(-10.4279896372952,0.389380420821346,
-2.27563934798683));
#29116=CARTESIAN_POINT('Ctrl Pts',(-10.3169681402164,2.12212224059811,-0.909257251928086));
#29117=CARTESIAN_POINT('Ctrl Pts',(-10.2059466431375,1.91618563379138,1.28778265676956));
#29118=CARTESIAN_POINT('Ctrl Pts',(-10.0949251460587,-0.0402946874592114,
2.30836043381174));
#29119=CARTESIAN_POINT('Ctrl Pts',(-9.98390364897989,-1.95996353772636,
1.22012068460793));
#29120=CARTESIAN_POINT('Ctrl Pts',(-9.87288215190107,-2.08909508774384,
-0.982768166247527));
#29121=CARTESIAN_POINT('Ctrl Pts',(-9.76186065482224,-0.309720379163782,
-2.28784283572006));
#29122=CARTESIAN_POINT('Ctrl Pts',(-9.65083915774341,1.75260137453506,-1.50284396269299));
#29123=CARTESIAN_POINT('Ctrl Pts',(-9.53981766066459,2.21382286633095,0.655087681715316));
#29124=CARTESIAN_POINT('Ctrl Pts',(-9.42879616358576,0.652592234905436,
2.2145597596737));
#29125=CARTESIAN_POINT('Ctrl Pts',(-9.31777466650695,-1.50481823148118,
1.75090652075626));
#29126=CARTESIAN_POINT('Ctrl Pts',(-9.2067531694281,-2.28749232053271,-0.31229863548985));
#29127=CARTESIAN_POINT('Ctrl Pts',(-9.0957316723493,-0.980413082489249,
-2.09020136396206));
#29128=CARTESIAN_POINT('Ctrl Pts',(-8.98471017527046,1.22232883501721,-1.95858718807982));
#29129=CARTESIAN_POINT('Ctrl Pts',(-8.87368867819164,2.30840438085843,-0.0376930850229031));
#29130=CARTESIAN_POINT('Ctrl Pts',(-8.76266718111281,1.28562225234641,1.91763577837313));
#29131=CARTESIAN_POINT('Ctrl Pts',(-8.65164568403398,-0.911648356460311,
2.12109613841244));
#29132=CARTESIAN_POINT('Ctrl Pts',(-8.54062418695517,-2.27607674369842,
0.386815474121903));
#29133=CARTESIAN_POINT('Ctrl Pts',(-8.42960268987633,-1.56118057750606,
-1.70084295531445));
#29134=CARTESIAN_POINT('Ctrl Pts',(-8.31858119279751,0.57994214986645,-2.23468535973931));
#29135=CARTESIAN_POINT('Ctrl Pts',(-8.20755969571868,2.19125499489417,-0.727016575860756));
#29136=CARTESIAN_POINT('Ctrl Pts',(-8.09653819863985,1.80073274085271,1.44482287850311));
#29137=CARTESIAN_POINT('Ctrl Pts',(-7.98551670156104,-0.234860494467263,
2.29673509625371));
#29138=CARTESIAN_POINT('Ctrl Pts',(-7.87449520448219,-2.05589541397972,
1.0504501896816));
#29139=CARTESIAN_POINT('Ctrl Pts',(-7.76347370740339,-1.99875385046778,
-1.1554802462462));
#29140=CARTESIAN_POINT('Ctrl Pts',(-7.65245221032454,-0.115637846925265,
-2.30581426888278));
#29141=CARTESIAN_POINT('Ctrl Pts',(-7.54143071324574,1.87311985568703,-1.34965683062618));
#29142=CARTESIAN_POINT('Ctrl Pts',(-7.43040921616689,2.15067686252692,0.839488288909578));
#29143=CARTESIAN_POINT('Ctrl Pts',(-7.31938771908808,0.46346918420048,2.2617134808639));
#29144=CARTESIAN_POINT('Ctrl Pts',(-7.20836622200924,-1.64714374930225,
1.61773577056313));
#29145=CARTESIAN_POINT('Ctrl Pts',(-7.09734472493043,-2.25299791294537,
-0.504134861409866));
#29146=CARTESIAN_POINT('Ctrl Pts',(-6.98632322785159,-0.800611337481142,
-2.16544984714991));
#29147=CARTESIAN_POINT('Ctrl Pts',(-6.87530173077277,1.38317887645369,-1.84850419257227));
#29148=CARTESIAN_POINT('Ctrl Pts',(-6.76428023369394,2.30335712846357,0.157154360362701));
#29149=CARTESIAN_POINT('Ctrl Pts',(-6.65325873661513,1.11928865601943,2.01924353626084));
#29150=CARTESIAN_POINT('Ctrl Pts',(-6.54223723953629,-1.08731316960842,
2.03663978784199));
#29151=CARTESIAN_POINT('Ctrl Pts',(-6.43121574245748,-2.30059305339287,
0.193450657547119));
#29152=CARTESIAN_POINT('Ctrl Pts',(-6.32019424537864,-1.41215135128814,
-1.82646656560694));
#29153=CARTESIAN_POINT('Ctrl Pts',(-6.20917274829982,0.766370303534781,
-2.17780350630744));
#29154=CARTESIAN_POINT('Ctrl Pts',(-6.09815125122099,2.24476943675482,-0.539594041883711));
#29155=CARTESIAN_POINT('Ctrl Pts',(-5.98712975414218,1.6724450082332,1.59156503123837));
#29156=CARTESIAN_POINT('Ctrl Pts',(-5.87610825706333,-0.427752318032092,
2.26873962998029));
#29157=CARTESIAN_POINT('Ctrl Pts',(-5.76508675998452,-2.13717376201072,
0.873292542735772));
#29158=CARTESIAN_POINT('Ctrl Pts',(-5.65406526290569,-1.89416636517823,
-1.3199565656689));
#29159=CARTESIAN_POINT('Ctrl Pts',(-5.54304376582687,0.0792689015851208,
-2.30735086093694));
#29160=CARTESIAN_POINT('Ctrl Pts',(-5.43202226874804,1.98028755329112,-1.18684993175432));
#29161=CARTESIAN_POINT('Ctrl Pts',(-5.32100077166922,2.072201769564,1.01790538874728));
#29162=CARTESIAN_POINT('Ctrl Pts',(-5.20997927459039,0.271042726753771,
2.29274669217924));
#29163=CARTESIAN_POINT('Ctrl Pts',(-5.09895777751157,-1.77772914296497,
1.47303450349202));
#29164=CARTESIAN_POINT('Ctrl Pts',(-4.98793628043274,-2.20244511626014,
-0.692377833330026));
#29165=CARTESIAN_POINT('Ctrl Pts',(-4.87691478335391,-0.615103183115273,
-2.22526394577057));
#29166=CARTESIAN_POINT('Ctrl Pts',(-4.76589328627509,1.53417022052411,-1.725245863256));
#29167=CARTESIAN_POINT('Ctrl Pts',(-4.65487178919626,2.28189254838822,0.350881677827793));
#29168=CARTESIAN_POINT('Ctrl Pts',(-4.54385029211743,0.944977257028757,
2.10645900456747));
#29169=CARTESIAN_POINT('Ctrl Pts',(-4.43282879503862,-1.25522808745102,
1.93766715477633));
#29170=CARTESIAN_POINT('Ctrl Pts',(-4.32180729795978,-2.3087117365316,-0.00129299116605801));
#29171=CARTESIAN_POINT('Ctrl Pts',(-4.21078580088096,-1.25305692450623,
-1.93907191670966));
#29172=CARTESIAN_POINT('Ctrl Pts',(-4.09976430380213,0.947336103040959,
-2.10539921679951));
#29173=CARTESIAN_POINT('Ctrl Pts',(-3.98874280672331,2.28228413851649,-0.348325516292812));
#29174=CARTESIAN_POINT('Ctrl Pts',(-3.87772130964448,1.5322368150876,1.7269632007418));
#29175=CARTESIAN_POINT('Ctrl Pts',(-3.76669981256566,-0.617595309141191,
2.22457357449704));
#29176=CARTESIAN_POINT('Ctrl Pts',(-3.65567831548683,-2.20321926510898,
0.689910446417216));
#29177=CARTESIAN_POINT('Ctrl Pts',(-3.54465681840801,-1.77607808597735,
-1.47502480885725));
#29178=CARTESIAN_POINT('Ctrl Pts',(-3.43363532132918,0.273610655848373,
-2.29244165972025));
#29179=CARTESIAN_POINT('Ctrl Pts',(-3.32261382425035,2.07334062261079,-1.01558368283841));
#29180=CARTESIAN_POINT('Ctrl Pts',(-3.21159232717153,1.97895692377789,1.18906730175907));
#29181=CARTESIAN_POINT('Ctrl Pts',(-3.1005708300927,0.0766843946343644,
2.30743820237117));
#29182=CARTESIAN_POINT('Ctrl Pts',(-2.98954933301387,-1.89564365655482,
1.31783408726441));
#29183=CARTESIAN_POINT('Ctrl Pts',(-2.87852783593505,-2.13619424888191,
-0.875685837292615));
#29184=CARTESIAN_POINT('Ctrl Pts',(-2.76750633885622,-0.425210840708204,
-2.2692173308279));
#29185=CARTESIAN_POINT('Ctrl Pts',(-2.6564848417774,1.67422666639024,-1.58969073211401));
#29186=CARTESIAN_POINT('Ctrl Pts',(-2.54546334469857,2.24416363123536,0.542108063755256));
#29187=CARTESIAN_POINT('Ctrl Pts',(-2.43444184761975,0.763930470417198,
2.1786605485489));
#29188=CARTESIAN_POINT('Ctrl Pts',(-2.32342035054092,-1.41419628399901,
1.8248836746595));
#29189=CARTESIAN_POINT('Ctrl Pts',(-2.2123988534621,-2.30037492951871,-0.196027426983243));
#29190=CARTESIAN_POINT('Ctrl Pts',(-2.10137735638327,-1.0850312476146,-2.0378564009861));
#29191=CARTESIAN_POINT('Ctrl Pts',(-1.99035585930445,1.12154969257803,-2.0179885682968));
#29192=CARTESIAN_POINT('Ctrl Pts',(-1.87933436222562,2.3035317313149,-0.154574257386218));
#29193=CARTESIAN_POINT('Ctrl Pts',(-1.76831286514679,1.38110746710851,1.85005228864688));
#29194=CARTESIAN_POINT('Ctrl Pts',(-1.65729136806797,-0.803036278516782,
2.16455180066113));
#29195=CARTESIAN_POINT('Ctrl Pts',(-1.54626987098914,-2.25356131479715,
0.501610826912889));
#29196=CARTESIAN_POINT('Ctrl Pts',(-1.43524837391032,-1.64533043758998,
-1.61957944731974));
#29197=CARTESIAN_POINT('Ctrl Pts',(-1.32422687683149,0.46600174301246,-2.26119344438801));
#29198=CARTESIAN_POINT('Ctrl Pts',(-1.21320537975266,2.15161675307334,-0.837077819272669));
#29199=CARTESIAN_POINT('Ctrl Pts',(-1.10218388267384,1.87160516180001,1.35175220315016));
#29200=CARTESIAN_POINT('Ctrl Pts',(-0.991162385595015,-0.118217138374247,
2.30568683075082));
#29201=CARTESIAN_POINT('Ctrl Pts',(-0.88014088851619,-2.00005326367194,
1.1532339979478));
#29202=CARTESIAN_POINT('Ctrl Pts',(-0.769119391437363,-2.05470530709598,
-1.0527395363478));
#29203=CARTESIAN_POINT('Ctrl Pts',(-0.65809789435854,-0.23231101724133,
-2.29702107407985));
#29204=CARTESIAN_POINT('Ctrl Pts',(-0.547076397279713,1.80239417156319,
-1.44275863580475));
#29205=CARTESIAN_POINT('Ctrl Pts',(-0.436054900200888,2.19035514254088,
0.729382352103237));
#29206=CARTESIAN_POINT('Ctrl Pts',(-0.325033403122062,0.577598884531914,
2.23550138713472));
#29207=CARTESIAN_POINT('Ctrl Pts',(-0.214011906043236,-1.56338978025347,
1.69877361619258));
#29208=CARTESIAN_POINT('Ctrl Pts',(-0.10299040896441,-2.27505899361857,
-0.388754641704208));
#29209=CARTESIAN_POINT('Ctrl Pts',(0.00803108811441417,-0.910403142496731,
-2.12329263712614));
#29210=CARTESIAN_POINT('Ctrl Pts',(0.119052585193242,1.29010742402986,-1.9138186660827));
#29211=CARTESIAN_POINT('Ctrl Pts',(0.193066916579125,1.96502654933667,-0.614881969531372));
#29212=CARTESIAN_POINT('Ctrl Pts',(0.230074082272067,1.95370260140122,0.0340902519511237));
#29213=CARTESIAN_POINT('',(0.,-0.896933272146831,-1.73598004173895));
#29214=CARTESIAN_POINT('Ctrl Pts',(2.66453525910038E-15,-0.897777576978214,
-1.73914455526119));
#29215=CARTESIAN_POINT('Ctrl Pts',(2.42885616950946E-15,-0.854308595888035,
-1.75665132687895));
#29216=CARTESIAN_POINT('Ctrl Pts',(-1.52008741663672E-16,-0.810233059137786,
-1.77245732638827));
#29217=CARTESIAN_POINT('Ctrl Pts',(8.60422844084496E-16,-0.765604712779606,
-1.78648174433319));
#29218=CARTESIAN_POINT('Ctrl Pts',(2.41466958929901E-15,-0.697057735880828,
-1.80802257054201));
#29219=CARTESIAN_POINT('Ctrl Pts',(3.66730899670521E-15,-0.627206169701796,
-1.82536276747026));
#29220=CARTESIAN_POINT('Ctrl Pts',(4.13558076672871E-15,-0.556420062791459,
-1.83857524845937));
#29221=CARTESIAN_POINT('Ctrl Pts',(4.36243855997318E-15,-0.522127199044321,
-1.84497613459506));
#29222=CARTESIAN_POINT('Ctrl Pts',(8.67308952147876E-15,-0.48761501095824,
-1.85040746202521));
#29223=CARTESIAN_POINT('Ctrl Pts',(9.43689570931383E-15,-0.452926237145203,
-1.85487325410974));
#29224=CARTESIAN_POINT('Ctrl Pts',(9.76107763911627E-15,-0.438203295885635,
-1.85676866831182));
#29225=CARTESIAN_POINT('Ctrl Pts',(6.11879014245653E-15,-0.423448554037784,
-1.85849011749958));
#29226=CARTESIAN_POINT('Ctrl Pts',(5.93969318174459E-15,-0.408665330346609,
-1.8600377655215));
#29227=CARTESIAN_POINT('Ctrl Pts',(5.75276829265403E-15,-0.393235964946499,
-1.86165305778386));
#29228=CARTESIAN_POINT('Ctrl Pts',(4.14358898742961E-15,-0.377783449474029,
-1.86307814468624));
#29229=CARTESIAN_POINT('Ctrl Pts',(4.19109191795997E-15,-0.36231842649289,
-1.86431332307229));
#29230=CARTESIAN_POINT('Ctrl Pts',(4.40966368558951E-15,-0.291160344840241,
-1.86999665924045));
#29231=CARTESIAN_POINT('Ctrl Pts',(3.34716857295974E-15,-0.219690647889499,
-1.87166839472062));
#29232=CARTESIAN_POINT('Ctrl Pts',(5.21804821573824E-15,-0.148275107848417,
-1.86939686799115));
#29233=CARTESIAN_POINT('Ctrl Pts',(6.55714620959737E-15,-0.0971588285257386,
-1.86777100344225));
#29234=CARTESIAN_POINT('Ctrl Pts',(1.54180173149947E-15,-0.0460702963087095,
-1.86412382836371));
#29235=CARTESIAN_POINT('Ctrl Pts',(1.33226762955019E-15,0.00485094964988812,
-1.85846491542322));
#29236=CARTESIAN_POINT('Ctrl Pts',(1.21176555987097E-15,0.0341355170380698,
-1.8552105013917));
#29237=CARTESIAN_POINT('Ctrl Pts',(4.62515714886742E-15,0.0633646503133136,
-1.8512905051685));
#29238=CARTESIAN_POINT('Ctrl Pts',(5.74540415243519E-15,0.0925106744803074,
-1.84670495503791));
#29239=CARTESIAN_POINT('Ctrl Pts',(6.22649828274991E-15,0.105027540050217,
-1.84473567393735));
#29240=CARTESIAN_POINT('Ctrl Pts',(5.83817128828971E-15,0.117520189266528,
-1.84264500601019));
#29241=CARTESIAN_POINT('Ctrl Pts',(5.6621374255883E-15,0.129983639985351,
-1.84043395959634));
#29242=CARTESIAN_POINT('Ctrl Pts',(4.69391821206743E-15,0.198534953167655,
-1.82827279022231));
#29243=CARTESIAN_POINT('Ctrl Pts',(4.42924793610523E-15,0.266233864746607,
-1.81246923639649));
#29244=CARTESIAN_POINT('Ctrl Pts',(4.413136522885E-15,0.332741006672829,
-1.7930834653544));
#29245=CARTESIAN_POINT('Ctrl Pts',(4.39742118597367E-15,0.397613164570649,
-1.7741742660776));
#29246=CARTESIAN_POINT('Ctrl Pts',(2.78842801225445E-15,0.461352264091458,
-1.75185630563892));
#29247=CARTESIAN_POINT('Ctrl Pts',(2.52575738102223E-15,0.52361861632967,
-1.72614358359088));
#29248=CARTESIAN_POINT('Ctrl Pts',(2.35257199225765E-15,0.564672396757043,
-1.70919053580173));
#29249=CARTESIAN_POINT('Ctrl Pts',(9.35783025048596E-16,0.605085429674089,
-1.69076091627867));
#29250=CARTESIAN_POINT('Ctrl Pts',(7.21644966006352E-16,0.644751661649001,
-1.67084992281155));
#29251=CARTESIAN_POINT('Ctrl Pts',(5.4073076524326E-16,0.678263615045427,
-1.65402815144772));
#29252=CARTESIAN_POINT('Ctrl Pts',(6.64449045267152E-15,0.711242437386654,
-1.63614889178973));
#29253=CARTESIAN_POINT('Ctrl Pts',(6.68909372336657E-15,0.743619323760163,
-1.6172057038497));
#29254=CARTESIAN_POINT('Ctrl Pts',(6.70260297825943E-15,0.753425501734138,
-1.61146826911952));
#29255=CARTESIAN_POINT('Ctrl Pts',(-4.4167704875882E-15,0.763176219215081,
-1.60563322846188));
#29256=CARTESIAN_POINT('Ctrl Pts',(-4.10782519111308E-15,0.772857613917434,
-1.5997079485001));
#29257=CARTESIAN_POINT('Ctrl Pts',(-2.33423005065088E-15,0.828436626748831,
-1.56569206327379));
#29258=CARTESIAN_POINT('Ctrl Pts',(5.3236200784477E-15,0.88183656846137,
-1.52864593801835));
#29259=CARTESIAN_POINT('Ctrl Pts',(4.05231403988182E-15,0.932748709480243,
-1.48859056817433));
#29260=CARTESIAN_POINT('Ctrl Pts',(3.67993039744611E-15,0.947661600587246,
-1.47685777994778));
#29261=CARTESIAN_POINT('Ctrl Pts',(-2.77500390110177E-15,0.962360807573884,
-1.46486655879511));
#29262=CARTESIAN_POINT('Ctrl Pts',(-2.52575738102223E-15,0.976837943247501,
-1.45261684628832));
#29263=CARTESIAN_POINT('Ctrl Pts',(-1.61095971371858E-15,1.02921122594054,
-1.40830161221923));
#29264=CARTESIAN_POINT('Ctrl Pts',(-1.20919530929667E-15,1.07868231006794,
-1.36060541153686));
#29265=CARTESIAN_POINT('Ctrl Pts',(-1.08246744900953E-15,1.12509528635148,
-1.30988296450997));
#29266=CARTESIAN_POINT('Ctrl Pts',(-9.67595445409575E-16,1.16716615827062,
-1.26390578866033));
#29267=CARTESIAN_POINT('Ctrl Pts',(4.18879340799465E-17,1.20672391844854,
-1.21544096567182));
#29268=CARTESIAN_POINT('Ctrl Pts',(1.01307850997046E-15,1.24361190857,-1.16474132238846));
#29269=CARTESIAN_POINT('Ctrl Pts',(1.19552438322947E-15,1.25054161087308,
-1.15521699119912));
#29270=CARTESIAN_POINT('Ctrl Pts',(2.90706964741059E-15,1.25737148574206,
-1.14562128847553));
#29271=CARTESIAN_POINT('Ctrl Pts',(2.84494650060196E-15,1.26409862962719,
-1.13595948716456));
#29272=CARTESIAN_POINT('Ctrl Pts',(2.50292880016366E-15,1.30113478121168,
-1.08276663979238));
#29273=CARTESIAN_POINT('Ctrl Pts',(1.91762847285502E-15,1.33508460122726,
-1.02753972970139));
#29274=CARTESIAN_POINT('Ctrl Pts',(2.04003480774873E-15,1.36583796777706,
-0.970591450617083));
#29275=CARTESIAN_POINT('Ctrl Pts',(2.16190419186033E-15,1.39645643081688,
-0.913892982320922));
#29276=CARTESIAN_POINT('Ctrl Pts',(-1.01931864381867E-15,1.42390663940794,
-0.855487109860612));
#29277=CARTESIAN_POINT('Ctrl Pts',(-3.59434704222394E-15,1.44803019585752,
-0.795670327485843));
#29278=CARTESIAN_POINT('Ctrl Pts',(-6.11597449534489E-15,1.47165347793389,
-0.737094025691661));
#29279=CARTESIAN_POINT('Ctrl Pts',(1.01337469259877E-15,1.4920867044338,
-0.677163760277832));
#29280=CARTESIAN_POINT('Ctrl Pts',(2.08166817117217E-16,1.5091315905072,
-0.616161567602637));
#29281=CARTESIAN_POINT('Ctrl Pts',(6.26169911362964E-17,1.51221263364822,
-0.605134777131891));
#29282=CARTESIAN_POINT('Ctrl Pts',(3.45179592633212E-16,1.5151828306955,
-0.594072993522759));
#29283=CARTESIAN_POINT('Ctrl Pts',(3.88578058618805E-16,1.51804083102399,
-0.582977932470115));
#29284=CARTESIAN_POINT('Ctrl Pts',(4.28030529389721E-16,1.52063896835125,
-0.572891687209135));
#29285=CARTESIAN_POINT('Ctrl Pts',(-1.01862452835985E-15,1.52314194434016,
-0.562787410979804));
#29286=CARTESIAN_POINT('Ctrl Pts',(-8.32667268468867E-16,1.52554925331476,
-0.552666456127963));
#29287=CARTESIAN_POINT('Ctrl Pts',(2.76065174993704E-16,1.53990234478933,
-0.492322315707556));
#29288=CARTESIAN_POINT('Ctrl Pts',(-3.91459791985415E-16,1.55085890343775,
-0.431384487161399));
#29289=CARTESIAN_POINT('Ctrl Pts',(3.01841884819964E-16,1.55828603425274,
-0.370123355547507));
#29290=CARTESIAN_POINT('Ctrl Pts',(9.825982558262E-16,1.56557877100754,
-0.309970745166737));
#29291=CARTESIAN_POINT('Ctrl Pts',(3.5825896615399E-15,1.56946866269597,
-0.24950554168674));
#29292=CARTESIAN_POINT('Ctrl Pts',(3.23005511226881E-15,1.56978073257091,
-0.188991307723295));
#29293=CARTESIAN_POINT('Ctrl Pts',(2.88873803673286E-15,1.57008287253789,
-0.130402606538099));
#29294=CARTESIAN_POINT('Ctrl Pts',(5.02537364202987E-15,1.56703113522227,
-0.0717672828486066));
#29295=CARTESIAN_POINT('Ctrl Pts',(6.32133234645949E-15,1.56042122340447,
-0.013342828381275));
#29296=CARTESIAN_POINT('Ctrl Pts',(6.62092093472987E-15,1.55889320083453,
0.000163234562326977));
#29297=CARTESIAN_POINT('Ctrl Pts',(2.18341315110387E-15,1.55717483559577,
0.0136579261245166));
#29298=CARTESIAN_POINT('Ctrl Pts',(2.22044604925031E-15,1.55526325306019,
0.0271378643347));
#29299=CARTESIAN_POINT('Ctrl Pts',(-0.121869692124238,-1.95503470185946,
-0.00140694303418273));
#29300=CARTESIAN_POINT('Ctrl Pts',(-0.115576597737629,-1.9560114957989,
-0.111573334849889));
#29301=CARTESIAN_POINT('Ctrl Pts',(-0.10928350335102,-1.9475116218801,-0.221598758420366));
#29302=CARTESIAN_POINT('Ctrl Pts',(-0.10299040896441,-1.92900481620408,
-0.329922931291736));
#29303=CARTESIAN_POINT('Ctrl Pts',(-0.0686602726429393,-1.82804634923992,
-0.920853782336577));
#29304=CARTESIAN_POINT('Ctrl Pts',(-0.0343301363214685,-1.42928869857895,
-1.46115662054476));
#29305=CARTESIAN_POINT('Ctrl Pts',(2.32452945780892E-15,-0.897777576978214,
-1.73914455526119));
#29306=CARTESIAN_POINT('',(-15.646,-0.903606778650182,-1.26612599672285));
#29307=CARTESIAN_POINT('Ctrl Pts',(-15.646,-0.90554130419335,-1.26787397308659));
#29308=CARTESIAN_POINT('Ctrl Pts',(-15.646,-0.9388319205117,-1.25008095488368));
#29309=CARTESIAN_POINT('Ctrl Pts',(-15.646,-0.971367568991014,-1.23102934423823));
#29310=CARTESIAN_POINT('Ctrl Pts',(-15.646,-1.0030683062222,-1.21073538899741));
#29311=CARTESIAN_POINT('Ctrl Pts',(-15.646,-1.05303568714615,-1.17874762213329));
#29312=CARTESIAN_POINT('Ctrl Pts',(-15.646,-1.10093004937321,-1.14367606433464));
#29313=CARTESIAN_POINT('Ctrl Pts',(-15.646,-1.14667319981616,-1.10584089641864));
#29314=CARTESIAN_POINT('Ctrl Pts',(-15.646,-1.17363908823249,-1.08353681577801));
#29315=CARTESIAN_POINT('Ctrl Pts',(-15.646,-1.1998571211457,-1.06027134077856));
#29316=CARTESIAN_POINT('Ctrl Pts',(-15.646,-1.22530816463228,-1.03610248194796));
#29317=CARTESIAN_POINT('Ctrl Pts',(-15.646,-1.23682022027328,-1.02517038606812));
#29318=CARTESIAN_POINT('Ctrl Pts',(-15.646,-1.24817682883917,-1.01405163699654));
#29319=CARTESIAN_POINT('Ctrl Pts',(-15.646,-1.25936010833055,-1.00276802411491));
#29320=CARTESIAN_POINT('Ctrl Pts',(-15.646,-1.30322784282822,-0.958506720045097));
#29321=CARTESIAN_POINT('Ctrl Pts',(-15.646,-1.34448541532842,-0.911661957910068));
#29322=CARTESIAN_POINT('Ctrl Pts',(-15.646,-1.38304512047716,-0.862582893866261));
#29323=CARTESIAN_POINT('Ctrl Pts',(-15.646,-1.41274047352769,-0.824786439548259));
#29324=CARTESIAN_POINT('Ctrl Pts',(-15.646,-1.44083552294601,-0.785663647481262));
#29325=CARTESIAN_POINT('Ctrl Pts',(-15.646,-1.4672800556148,-0.745355620103979));
#29326=CARTESIAN_POINT('Ctrl Pts',(-15.646,-1.47638184737574,-0.731482231752685));
#29327=CARTESIAN_POINT('Ctrl Pts',(-15.646,-1.48528802466688,-0.717468314833474));
#29328=CARTESIAN_POINT('Ctrl Pts',(-15.646,-1.4939962396742,-0.70331926166881));
#29329=CARTESIAN_POINT('Ctrl Pts',(-15.646,-1.50231026779888,-0.689810680880463));
#29330=CARTESIAN_POINT('Ctrl Pts',(-15.646,-1.51044565988147,-0.676175502864343));
#29331=CARTESIAN_POINT('Ctrl Pts',(-15.646,-1.5183869558134,-0.662442089798388));
#29332=CARTESIAN_POINT('Ctrl Pts',(-15.646,-1.55077996339743,-0.606422699838139));
#29333=CARTESIAN_POINT('Ctrl Pts',(-15.646,-1.57999117124514,-0.548701659160568));
#29334=CARTESIAN_POINT('Ctrl Pts',(-15.646,-1.60592950648782,-0.489633408577941));
#29335=CARTESIAN_POINT('Ctrl Pts',(-15.646,-1.6324092676445,-0.429332192145295));
#29336=CARTESIAN_POINT('Ctrl Pts',(-15.646,-1.65547885224142,-0.367626155535072));
#29337=CARTESIAN_POINT('Ctrl Pts',(-15.646,-1.67500744714839,-0.304850769250659));
#29338=CARTESIAN_POINT('Ctrl Pts',(-15.646,-1.68791747427872,-0.263351012411529));
#29339=CARTESIAN_POINT('Ctrl Pts',(-15.646,-1.69927926283844,-0.221383073699382));
#29340=CARTESIAN_POINT('Ctrl Pts',(-15.646,-1.70904465268481,-0.179036877539802));
#29341=CARTESIAN_POINT('Ctrl Pts',(-15.646,-1.71384145896988,-0.158236223077195));
#29342=CARTESIAN_POINT('Ctrl Pts',(-15.646,-1.71825294582739,-0.137344232813234));
#29343=CARTESIAN_POINT('Ctrl Pts',(-15.646,-1.72227256103369,-0.116371238196171));
#29344=CARTESIAN_POINT('Ctrl Pts',(-15.646,-1.72482838629632,-0.103035805144933));
#29345=CARTESIAN_POINT('Ctrl Pts',(-15.646,-1.72722577012393,-0.0896676190078338));
#29346=CARTESIAN_POINT('Ctrl Pts',(-15.646,-1.72946290153931,-0.0762693043065953));
#29347=CARTESIAN_POINT('Ctrl Pts',(-15.646,-1.73118679540451,-0.065944800185506));
#29348=CARTESIAN_POINT('Ctrl Pts',(-15.646,-1.73281491882756,-0.0556057409752924));
#29349=CARTESIAN_POINT('Ctrl Pts',(-15.646,-1.73434548980575,-0.045261864309701));
#29350=CARTESIAN_POINT('Ctrl Pts',(-15.646,-1.74426354163551,0.0217661313542963));
#29351=CARTESIAN_POINT('Ctrl Pts',(-15.646,-1.75010629770909,0.0890975130769489));
#29352=CARTESIAN_POINT('Ctrl Pts',(-15.646,-1.75175066215845,0.156377409541393));
#29353=CARTESIAN_POINT('Ctrl Pts',(-15.646,-1.75216844738295,0.173471276208168));
#29354=CARTESIAN_POINT('Ctrl Pts',(-15.646,-1.75231500242569,0.190561969387215));
#29355=CARTESIAN_POINT('Ctrl Pts',(-15.646,-1.75218784680546,0.207643941770755));
#29356=CARTESIAN_POINT('Ctrl Pts',(-15.646,-1.7517050717956,0.272499505144288));
#29357=CARTESIAN_POINT('Ctrl Pts',(-15.646,-1.74728083397727,0.337228600758688));
#29358=CARTESIAN_POINT('Ctrl Pts',(-15.646,-1.73913184783819,0.401595905267991));
#29359=CARTESIAN_POINT('Ctrl Pts',(-15.646,-1.73471144430273,0.436511839049797));
#29360=CARTESIAN_POINT('Ctrl Pts',(-15.646,-1.72919412473302,0.47132150623283));
#29361=CARTESIAN_POINT('Ctrl Pts',(-15.646,-1.72260827310355,0.505987965615567));
#29362=CARTESIAN_POINT('Ctrl Pts',(-15.646,-1.71757351777636,0.532489798768173));
#29363=CARTESIAN_POINT('Ctrl Pts',(-15.646,-1.71191419079661,0.558907947509954));
#29364=CARTESIAN_POINT('Ctrl Pts',(-15.646,-1.70564134060446,0.585225824611134));
#29365=CARTESIAN_POINT('Ctrl Pts',(-15.646,-1.70220225814383,0.599654568605839));
#29366=CARTESIAN_POINT('Ctrl Pts',(-15.646,-1.69857761981803,0.614056894407544));
#29367=CARTESIAN_POINT('Ctrl Pts',(-15.646,-1.69477643427966,0.628403772607706));
#29368=CARTESIAN_POINT('Ctrl Pts',(-15.646,-1.67740647456813,0.693963502278271));
#29369=CARTESIAN_POINT('Ctrl Pts',(-15.646,-1.65633175680869,0.758467910098477));
#29370=CARTESIAN_POINT('Ctrl Pts',(-15.646,-1.63180977190725,0.821661415923179));
#29371=CARTESIAN_POINT('Ctrl Pts',(-15.646,-1.60677175649931,0.886184739743799));
#29372=CARTESIAN_POINT('Ctrl Pts',(-15.646,-1.57813969140247,0.949342287961683));
#29373=CARTESIAN_POINT('Ctrl Pts',(-15.646,-1.546132490592,1.01086511111923));
#29374=CARTESIAN_POINT('Ctrl Pts',(-15.646,-1.51388293863644,1.07285377090927));
#29375=CARTESIAN_POINT('Ctrl Pts',(-15.646,-1.47820662246953,1.1331838390446));
#29376=CARTESIAN_POINT('Ctrl Pts',(-15.646,-1.43927596686557,1.19156917309334));
#29377=CARTESIAN_POINT('Ctrl Pts',(-15.646,-1.4294481205191,1.20630825423689));
#29378=CARTESIAN_POINT('Ctrl Pts',(-15.646,-1.41941263972777,1.22092330393712));
#29379=CARTESIAN_POINT('Ctrl Pts',(-15.646,-1.40917182388351,1.23540949097454));
#29380=CARTESIAN_POINT('Ctrl Pts',(-15.646,-1.40170116694523,1.24597713864501));
#29381=CARTESIAN_POINT('Ctrl Pts',(-15.646,-1.39412021842425,1.25647742423705));
#29382=CARTESIAN_POINT('Ctrl Pts',(-15.646,-1.3864413518955,1.26689325751344));
#29383=CARTESIAN_POINT('Ctrl Pts',(-15.646,-1.34360456056451,1.3249983013931));
#29384=CARTESIAN_POINT('Ctrl Pts',(-15.646,-1.29765039571163,1.38058334275533));
#29385=CARTESIAN_POINT('Ctrl Pts',(-15.646,-1.24882029809218,1.43336797698167));
#29386=CARTESIAN_POINT('Ctrl Pts',(-15.646,-1.19987423803885,1.48627796493359));
#29387=CARTESIAN_POINT('Ctrl Pts',(-15.646,-1.14803813754689,1.53637523807351));
#29388=CARTESIAN_POINT('Ctrl Pts',(-15.646,-1.09350553802909,1.58336120199917));
#29389=CARTESIAN_POINT('Ctrl Pts',(-15.646,-1.04013426283505,1.62934655448756));
#29390=CARTESIAN_POINT('Ctrl Pts',(-15.646,-0.984179545234824,1.6723525600043));
#29391=CARTESIAN_POINT('Ctrl Pts',(-15.646,-0.925783035097312,1.71207017058232));
#29392=CARTESIAN_POINT('Ctrl Pts',(-15.646,-0.904681296506683,1.72642223775017));
#29393=CARTESIAN_POINT('Ctrl Pts',(-15.646,-0.883260377259073,1.74034457784343));
#29394=CARTESIAN_POINT('Ctrl Pts',(-15.646,-0.861525859670562,1.75382131162753));
#29395=CARTESIAN_POINT('Ctrl Pts',(-15.646,-0.905541304193346,-1.2678739730866));
#29396=CARTESIAN_POINT('Ctrl Pts',(-15.6116698636785,-0.515499657429897,
-1.54330953138525));
#29397=CARTESIAN_POINT('Ctrl Pts',(-15.5403325616641,0.580821856359331,
-1.72219244777323));
#29398=CARTESIAN_POINT('Ctrl Pts',(-15.4319880939568,1.77133009557791,-0.489978596140976));
#29399=CARTESIAN_POINT('Ctrl Pts',(-15.3209665968779,1.37345033995276,1.2214745163176));
#29400=CARTESIAN_POINT('Ctrl Pts',(-15.2099450997991,-0.279367108572254,
1.81642835228867));
#29401=CARTESIAN_POINT('Ctrl Pts',(-15.1202708256386,-1.40814580884089,
0.95690627970636));
#29402=CARTESIAN_POINT('Ctrl Pts',(-15.067603717171,-1.55400039997039,0.220042953926479));
#29403=CARTESIAN_POINT('Ctrl Pts',(-15.0519437743963,-1.55320111767851,
0.000640865722738825));
#29404=CARTESIAN_POINT('Origin',(-15.646,-2.59090492670967E-16,0.));
#29405=CARTESIAN_POINT('',(-15.646,-1.954,-2.39295984553393E-16));
#29406=CARTESIAN_POINT('Origin',(-15.646,0.,0.));
#29407=CARTESIAN_POINT('Origin',(-15.646,0.,0.));
#29408=CARTESIAN_POINT('',(-15.646,0.903606778650233,-1.26612599672282));
#29409=CARTESIAN_POINT('Ctrl Pts',(-15.646,0.863566983235665,1.75638267756862));
#29410=CARTESIAN_POINT('Ctrl Pts',(-15.646,0.903502374498014,1.73186322492154));
#29411=CARTESIAN_POINT('Ctrl Pts',(-15.646,0.942431754046728,1.7058442816782));
#29412=CARTESIAN_POINT('Ctrl Pts',(-15.646,0.980258194321091,1.67832096079393));
#29413=CARTESIAN_POINT('Ctrl Pts',(-15.646,1.03835777356149,1.6360464736607));
#29414=CARTESIAN_POINT('Ctrl Pts',(-15.646,1.09385752849377,1.59022401101361));
#29415=CARTESIAN_POINT('Ctrl Pts',(-15.646,1.14659587359059,1.54119436771133));
#29416=CARTESIAN_POINT('Ctrl Pts',(-15.646,1.17214536647838,1.5174415836499));
#29417=CARTESIAN_POINT('Ctrl Pts',(-15.646,1.19704611900917,1.49293561765741));
#29418=CARTESIAN_POINT('Ctrl Pts',(-15.646,1.22127593441469,1.46771321296535));
#29419=CARTESIAN_POINT('Ctrl Pts',(-15.646,1.23155978876183,1.45700807420153));
#29420=CARTESIAN_POINT('Ctrl Pts',(-15.646,1.24172274779762,1.44617386383036));
#29421=CARTESIAN_POINT('Ctrl Pts',(-15.646,1.25176296848256,1.43521334664126));
#29422=CARTESIAN_POINT('Ctrl Pts',(-15.646,1.26224201312144,1.42377378246295));
#29423=CARTESIAN_POINT('Ctrl Pts',(-15.646,1.27258196295285,1.41220243610557));
#29424=CARTESIAN_POINT('Ctrl Pts',(-15.646,1.28277672403329,1.40050803765028));
#29425=CARTESIAN_POINT('Ctrl Pts',(-15.646,1.32968516061639,1.34669942516889));
#29426=CARTESIAN_POINT('Ctrl Pts',(-15.646,1.37355485596852,1.2902533722939));
#29427=CARTESIAN_POINT('Ctrl Pts',(-15.646,1.41422309221843,1.23150451481102));
#29428=CARTESIAN_POINT('Ctrl Pts',(-15.646,1.44333172695657,1.18945452220145));
#29429=CARTESIAN_POINT('Ctrl Pts',(-15.646,1.4707993065757,1.14622410435876));
#29430=CARTESIAN_POINT('Ctrl Pts',(-15.646,1.49655049600041,1.10193110550949));
#29431=CARTESIAN_POINT('Ctrl Pts',(-15.646,1.51135988777298,1.07645840357241));
#29432=CARTESIAN_POINT('Ctrl Pts',(-15.646,1.52560136048139,1.05063421753584));
#29433=CARTESIAN_POINT('Ctrl Pts',(-15.646,1.53925846964067,1.02448080677582));
#29434=CARTESIAN_POINT('Ctrl Pts',(-15.646,1.54512355904191,1.01324914050839));
#29435=CARTESIAN_POINT('Ctrl Pts',(-15.646,1.55087667965087,1.00196470925521));
#29436=CARTESIAN_POINT('Ctrl Pts',(-15.646,1.5565156774274,0.990632117118322));
#29437=CARTESIAN_POINT('Ctrl Pts',(-15.646,1.58753124253106,0.928300695269239));
#29438=CARTESIAN_POINT('Ctrl Pts',(-15.646,1.61511219349458,0.864487052005008));
#29439=CARTESIAN_POINT('Ctrl Pts',(-15.646,1.63910495617291,0.799499739891529));
#29440=CARTESIAN_POINT('Ctrl Pts',(-15.646,1.66250789621328,0.736110034038682));
#29441=CARTESIAN_POINT('Ctrl Pts',(-15.646,1.68249698900462,0.671602682530926));
#29442=CARTESIAN_POINT('Ctrl Pts',(-15.646,1.69888136394285,0.606259025222021));
#29443=CARTESIAN_POINT('Ctrl Pts',(-15.646,1.70968399200845,0.56317631812975));
#29444=CARTESIAN_POINT('Ctrl Pts',(-15.646,1.71891862839643,0.519729989653583));
#29445=CARTESIAN_POINT('Ctrl Pts',(-15.646,1.72651830953887,0.476002417985191));
#29446=CARTESIAN_POINT('Ctrl Pts',(-15.646,1.73293889141712,0.439059229320861));
#29447=CARTESIAN_POINT('Ctrl Pts',(-15.646,1.73819233547822,0.401915291206649));
#29448=CARTESIAN_POINT('Ctrl Pts',(-15.646,1.74223252542586,0.364622070603487));
#29449=CARTESIAN_POINT('Ctrl Pts',(-15.646,1.74345619948668,0.353326872286555));
#29450=CARTESIAN_POINT('Ctrl Pts',(-15.646,1.74456842691372,0.342018170207851));
#29451=CARTESIAN_POINT('Ctrl Pts',(-15.646,1.74556687996462,0.330711488807271));
#29452=CARTESIAN_POINT('Ctrl Pts',(-15.646,1.75129881468264,0.265801917338621));
#29453=CARTESIAN_POINT('Ctrl Pts',(-15.646,1.75329872256676,0.200840616042056));
#29454=CARTESIAN_POINT('Ctrl Pts',(-15.646,1.7513997771477,0.136088205278388));
#29455=CARTESIAN_POINT('Ctrl Pts',(-15.646,1.75084355022554,0.117121344103708));
#29456=CARTESIAN_POINT('Ctrl Pts',(-15.646,1.74995247314858,0.0981724485182577));
#29457=CARTESIAN_POINT('Ctrl Pts',(-15.646,1.74872150843178,0.0792482245434431));
#29458=CARTESIAN_POINT('Ctrl Pts',(-15.646,1.7442682940956,0.0107867777160483));
#29459=CARTESIAN_POINT('Ctrl Pts',(-15.646,1.73537089691159,-0.0573539081323246));
#29460=CARTESIAN_POINT('Ctrl Pts',(-15.646,1.72222163795807,-0.124837458918125));
#29461=CARTESIAN_POINT('Ctrl Pts',(-15.646,1.7103025383206,-0.186007686727107));
#29462=CARTESIAN_POINT('Ctrl Pts',(-15.646,1.69488873716282,-0.24663831729391));
#29463=CARTESIAN_POINT('Ctrl Pts',(-15.646,1.67609021756689,-0.306453003759262));
#29464=CARTESIAN_POINT('Ctrl Pts',(-15.646,1.67255876966726,-0.317689657146101));
#29465=CARTESIAN_POINT('Ctrl Pts',(-15.646,1.66891056048996,-0.328888546226132));
#29466=CARTESIAN_POINT('Ctrl Pts',(-15.646,1.6651481002395,-0.340044199921187));
#29467=CARTESIAN_POINT('Ctrl Pts',(-15.646,1.64443393500422,-0.401461474407603));
#29468=CARTESIAN_POINT('Ctrl Pts',(-15.646,1.62024853883519,-0.461608555356997));
#29469=CARTESIAN_POINT('Ctrl Pts',(-15.646,1.5927777004272,-0.520210875318301));
#29470=CARTESIAN_POINT('Ctrl Pts',(-15.646,1.56542737352935,-0.578556113425322));
#29471=CARTESIAN_POINT('Ctrl Pts',(-15.646,1.53481960882925,-0.635370945735342));
#29472=CARTESIAN_POINT('Ctrl Pts',(-15.646,1.50109845003964,-0.690351644448425));
#29473=CARTESIAN_POINT('Ctrl Pts',(-15.646,1.46807660782277,-0.744192141722088));
#29474=CARTESIAN_POINT('Ctrl Pts',(-15.646,1.43206841909097,-0.796274405573291));
#29475=CARTESIAN_POINT('Ctrl Pts',(-15.646,1.3931825738236,-0.846271253612836));
#29476=CARTESIAN_POINT('Ctrl Pts',(-15.646,1.38615361009627,-0.855308630296688));
#29477=CARTESIAN_POINT('Ctrl Pts',(-15.646,1.37903056784112,-0.864277742013307));
#29478=CARTESIAN_POINT('Ctrl Pts',(-15.646,1.37181402230227,-0.873176482427014));
#29479=CARTESIAN_POINT('Ctrl Pts',(-15.646,1.36525350796304,-0.881266269122166));
#29480=CARTESIAN_POINT('Ctrl Pts',(-15.646,1.35862187689793,-0.889290301674277));
#29481=CARTESIAN_POINT('Ctrl Pts',(-15.646,1.35191991563543,-0.897247368324002));
#29482=CARTESIAN_POINT('Ctrl Pts',(-15.646,1.31196126683496,-0.944689246795767));
#29483=CARTESIAN_POINT('Ctrl Pts',(-15.646,1.26950445045268,-0.989754560841547));
#29484=CARTESIAN_POINT('Ctrl Pts',(-15.646,1.22468770075641,-1.03217561515895));
#29485=CARTESIAN_POINT('Ctrl Pts',(-15.646,1.18068191727077,-1.07382905375448));
#29486=CARTESIAN_POINT('Ctrl Pts',(-15.646,1.13440012852228,-1.11293359637472));
#29487=CARTESIAN_POINT('Ctrl Pts',(-15.646,1.08595004589958,-1.14919178596454));
#29488=CARTESIAN_POINT('Ctrl Pts',(-15.646,1.03904162600828,-1.18429625410389));
#29489=CARTESIAN_POINT('Ctrl Pts',(-15.646,0.990100100246089,-1.21673292322258));
#29490=CARTESIAN_POINT('Ctrl Pts',(-15.646,0.939210854429017,-1.24618438366542));
#29491=CARTESIAN_POINT('Ctrl Pts',(-15.646,0.927446614173192,-1.25299277807118));
#29492=CARTESIAN_POINT('Ctrl Pts',(-15.646,0.915578253025946,-1.25964142336886));
#29493=CARTESIAN_POINT('Ctrl Pts',(-15.646,0.903606778650246,-1.26612599672281));
#29494=CARTESIAN_POINT('Origin',(-15.646,0.,0.));
#29495=CARTESIAN_POINT('Origin',(-16.9400562256037,0.,0.));
#29496=CARTESIAN_POINT('Ctrl Pts',(-15.646,0.903606778650232,-1.26612599672282));
#29497=CARTESIAN_POINT('Ctrl Pts',(-15.6089928343071,1.32418286847098,-0.965969924828001));
#29498=CARTESIAN_POINT('Ctrl Pts',(-15.5349785029212,1.83555016250808,0.0811162878112121));
#29499=CARTESIAN_POINT('Ctrl Pts',(-15.4239570058423,0.927248239037281,
1.58822321403664));
#29500=CARTESIAN_POINT('Ctrl Pts',(-15.3129355087635,-0.828910895913401,
1.63972535647931));
#29501=CARTESIAN_POINT('Ctrl Pts',(-15.2349685820173,-1.53012672072011,
0.625555336487783));
#29502=CARTESIAN_POINT('Ctrl Pts',(-15.194008820964,-1.55770177041248,0.0560323151841793));
#29503=CARTESIAN_POINT('Ctrl Pts',(-15.1900562256037,-1.55731346481242,
0.00103325697183652));
#29504=CARTESIAN_POINT('Ctrl Pts',(-15.8760740822721,1.13509973994377,-1.59049193030949));
#29505=CARTESIAN_POINT('Ctrl Pts',(-15.8390669165791,1.66342225971859,-1.21343955841462));
#29506=CARTESIAN_POINT('Ctrl Pts',(-15.7650525851932,2.30579557540391,0.101897284720716));
#29507=CARTESIAN_POINT('Ctrl Pts',(-15.6540310881144,1.16479785218828,1.99510649966415));
#29508=CARTESIAN_POINT('Ctrl Pts',(-15.5430095910356,-1.04126768924124,
2.05980285860533));
#29509=CARTESIAN_POINT('Ctrl Pts',(-15.4319880939568,-2.29557200334843,
0.245699716161034));
#29510=CARTESIAN_POINT('Ctrl Pts',(-15.3209665968779,-1.45300688747799,
-1.79439621415821));
#29511=CARTESIAN_POINT('Ctrl Pts',(-15.2099450997991,0.717101347881572,
-2.19440670210365));
#29512=CARTESIAN_POINT('Ctrl Pts',(-15.0989236027203,2.23202382251325,-0.590124666540823));
#29513=CARTESIAN_POINT('Ctrl Pts',(-14.9879021056415,1.70790504136699,1.55349118140293));
#29514=CARTESIAN_POINT('Ctrl Pts',(-14.8768806085626,-0.376501591705209,
2.27778871648529));
#29515=CARTESIAN_POINT('Ctrl Pts',(-14.7658591114838,-2.11694215263163,
0.921258901245484));
#29516=CARTESIAN_POINT('Ctrl Pts',(-14.654837614405,-1.92344217019805,-1.27692506070559));
#29517=CARTESIAN_POINT('Ctrl Pts',(-14.5438161173262,0.0272337144496871,
-2.30854902471789));
#29518=CARTESIAN_POINT('Ctrl Pts',(-14.4327946202473,1.95302852331423,-1.2311920503561));
#29519=CARTESIAN_POINT('Ctrl Pts',(-14.3217731231685,2.09462236852777,0.970933007055954));
#29520=CARTESIAN_POINT('Ctrl Pts',(-14.2107516260897,0.322660046842802,
2.28605351825641));
#29521=CARTESIAN_POINT('Ctrl Pts',(-14.0997301290109,-1.74407021311087,
1.5127364171163));
#29522=CARTESIAN_POINT('Ctrl Pts',(-13.988708631932,-2.21749402601248,-0.642551447391479));
#29523=CARTESIAN_POINT('Ctrl Pts',(-13.8776871348532,-0.665111842436208,
-2.21083194745943));
#29524=CARTESIAN_POINT('Ctrl Pts',(-13.7666656377744,1.49488751168712,-1.75939288428676));
#29525=CARTESIAN_POINT('Ctrl Pts',(-13.6556441406956,2.28922277847452,0.299350966372687));
#29526=CARTESIAN_POINT('Ctrl Pts',(-13.5446226436167,0.992223838228365,
2.0846207641111));
#29527=CARTESIAN_POINT('Ctrl Pts',(-13.4336011465379,-1.21122756867257,
1.96547187749358));
#29528=CARTESIAN_POINT('Ctrl Pts',(-13.3225796494591,-2.30815423967428,
0.0507534971524391));
#29529=CARTESIAN_POINT('Ctrl Pts',(-13.2115581523803,-1.29645175311226,
-1.91033105957732));
#29530=CARTESIAN_POINT('Ctrl Pts',(-13.1005366553014,0.89963257316349,-2.12622038973593));
#29531=CARTESIAN_POINT('Ctrl Pts',(-12.9895151582226,2.27385177436925,-0.399687400733145));
#29532=CARTESIAN_POINT('Ctrl Pts',(-12.8784936611438,1.57077905700222,1.69198258370345));
#29533=CARTESIAN_POINT('Ctrl Pts',(-12.767472164065,-0.56728897414607,2.23793099319152));
#29534=CARTESIAN_POINT('Ctrl Pts',(-12.6564506669861,-2.18710651309118,
0.739403144753916));
#29535=CARTESIAN_POINT('Ctrl Pts',(-12.5454291699073,-1.80887882518214,
-1.43461120371879));
#29536=CARTESIAN_POINT('Ctrl Pts',(-12.4344076728285,0.221861751741927,
-2.29802725686185));
#29537=CARTESIAN_POINT('Ctrl Pts',(-12.3233861757497,2.04991909791636,-1.06206572400144));
#29538=CARTESIAN_POINT('Ctrl Pts',(-12.2123646786708,2.00525966305359,1.14415278430378));
#29539=CARTESIAN_POINT('Ctrl Pts',(-12.101343181592,0.128682361216318,2.30512315506791));
#29540=CARTESIAN_POINT('Ctrl Pts',(-11.9903216845132,-1.86545353965054,
1.36023343640473));
#29541=CARTESIAN_POINT('Ctrl Pts',(-11.8793001874344,-2.15539235708442,
-0.827306289792927));
#29542=CARTESIAN_POINT('Ctrl Pts',(-11.7682786903555,-0.476258618959912,
-2.2590550320826));
#29543=CARTESIAN_POINT('Ctrl Pts',(-11.6572571932767,1.63796424475246,-1.62702951510483));
#29544=CARTESIAN_POINT('Ctrl Pts',(-11.5462356961979,2.25581433404732,0.491379283666496));
#29545=CARTESIAN_POINT('Ctrl Pts',(-11.435214199119,0.812850724616405,2.16088537632167));
#29546=CARTESIAN_POINT('Ctrl Pts',(-11.3241927020402,-1.37269789415048,
1.85630073035186));
#29547=CARTESIAN_POINT('Ctrl Pts',(-11.2131712049614,-2.30420951980991,
-0.144119391226494));
#29548=CARTESIAN_POINT('Ctrl Pts',(-11.1021497078826,-1.13069571341659,
-2.01287831568912));
#29549=CARTESIAN_POINT('Ctrl Pts',(-10.9911282108037,1.07577243683834,-2.04275930404171));
#29550=CARTESIAN_POINT('Ctrl Pts',(-10.8801067137249,2.2994617559248,-0.206464387121221));
#29551=CARTESIAN_POINT('Ctrl Pts',(-10.7690852166461,1.42246299320277,1.81844739904093));
#29552=CARTESIAN_POINT('Ctrl Pts',(-10.6580637195673,-0.75403598905343,
2.18210486396101));
#29553=CARTESIAN_POINT('Ctrl Pts',(-10.5470422224884,-2.24168054205987,
0.552286390797627));
#29554=CARTESIAN_POINT('Ctrl Pts',(-10.4360207254096,-1.68142341294711,
-1.58207686807671));
#29555=CARTESIAN_POINT('Ctrl Pts',(-10.3249992283308,0.414908893302569,
-2.27112362507384));
#29556=CARTESIAN_POINT('Ctrl Pts',(-10.213977731252,2.13219851056152,-0.885370782028248));
#29557=CARTESIAN_POINT('Ctrl Pts',(-10.1029562341731,1.90160445998143,1.30921823539425));
#29558=CARTESIAN_POINT('Ctrl Pts',(-9.99193473709432,-0.0662125798935141,
2.30776251039268));
#29559=CARTESIAN_POINT('Ctrl Pts',(-9.88091324001547,-1.97354069139653,
1.19803549593164));
#29560=CARTESIAN_POINT('Ctrl Pts',(-9.76989174293666,-2.07792800655941,
-1.00616455397024));
#29561=CARTESIAN_POINT('Ctrl Pts',(-9.65887024585783,-0.284010821989528,
-2.29117650195329));
#29562=CARTESIAN_POINT('Ctrl Pts',(-9.54784874877901,1.7693662763279,-1.48306941520065));
#29563=CARTESIAN_POINT('Ctrl Pts',(-9.43682725170018,2.20632742884456,0.679905277842615));
#29564=CARTESIAN_POINT('Ctrl Pts',(-9.32580575462136,0.62768396328097,2.22174812981805));
#29565=CARTESIAN_POINT('Ctrl Pts',(-9.21478425754252,-1.52438422544196,
1.73389868312246));
#29566=CARTESIAN_POINT('Ctrl Pts',(-9.10376276046371,-2.28384139715977,
-0.337965061403401));
#29567=CARTESIAN_POINT('Ctrl Pts',(-8.99274126338487,-0.956880566319905,
-2.10107864962485));
#29568=CARTESIAN_POINT('Ctrl Pts',(-8.88171976630606,1.24424466242879,-1.94473831919042));
#29569=CARTESIAN_POINT('Ctrl Pts',(-8.77069826922723,2.30868217437448,-0.0117697848585148));
#29570=CARTESIAN_POINT('Ctrl Pts',(-8.6596767721484,1.26400823191302,1.9319511121574));
#29571=CARTESIAN_POINT('Ctrl Pts',(-8.54865527506958,-0.935408563412113,
2.11072564053346));
#29572=CARTESIAN_POINT('Ctrl Pts',(-8.43763377799075,-2.28027684723519,
0.361233179640555));
#29573=CARTESIAN_POINT('Ctrl Pts',(-8.32661228091193,-1.54198354601843,
-1.71826617667884));
#29574=CARTESIAN_POINT('Ctrl Pts',(-8.2155907838331,0.604998744749697,-2.22803241200872));
#29575=CARTESIAN_POINT('Ctrl Pts',(-8.10456928675428,2.1992805397039,-0.702365302239374));
#29576=CARTESIAN_POINT('Ctrl Pts',(-7.99354778967544,1.78439544749182,1.46495214839276));
#29577=CARTESIAN_POINT('Ctrl Pts',(-7.88252629259663,-0.260635586535173,
2.29395313839267));
#29578=CARTESIAN_POINT('Ctrl Pts',(-7.77150479551778,-2.06756130355966,
1.02729847957288));
#29579=CARTESIAN_POINT('Ctrl Pts',(-7.66048329843898,-1.98565308907595,
-1.1778513148752));
#29580=CARTESIAN_POINT('Ctrl Pts',(-7.54946180136014,-0.0897387194211616,
-2.30696746235112));
#29581=CARTESIAN_POINT('Ctrl Pts',(-7.43844030428132,1.88815703473765,-1.32853864162123));
#29582=CARTESIAN_POINT('Ctrl Pts',(-7.3274188072025,2.1411147814535,0.863585202948405));
#29583=CARTESIAN_POINT('Ctrl Pts',(-7.21639731012367,0.438043343689854,
2.26677522907745));
#29584=CARTESIAN_POINT('Ctrl Pts',(-7.10537581304484,-1.66520540906234,
1.59913816030374));
#29585=CARTESIAN_POINT('Ctrl Pts',(-6.99435431596602,-2.24719504647279,
-0.529401863633136));
#29586=CARTESIAN_POINT('Ctrl Pts',(-6.88333281888719,-0.776245190777431,
-2.17430340888869));
#29587=CARTESIAN_POINT('Ctrl Pts',(-6.77231132180837,1.40384845329613,-1.83285608553649));
#29588=CARTESIAN_POINT('Ctrl Pts',(-6.66128982472955,2.30144731053276,0.183008707310951));
#29589=CARTESIAN_POINT('Ctrl Pts',(-6.5502683276507,1.09654416977377,2.03168471812071));
#29590=CARTESIAN_POINT('Ctrl Pts',(-6.4392468305719,-1.1101139524217,2.02430208287913));
#29591=CARTESIAN_POINT('Ctrl Pts',(-6.32822533349305,-2.302620330935,0.16760525551085));
#29592=CARTESIAN_POINT('Ctrl Pts',(-6.21720383641425,-1.39155309111705,
-1.84220843139767));
#29593=CARTESIAN_POINT('Ctrl Pts',(-6.10618233933541,0.790776428311071,
-2.16906075307671));
#29594=CARTESIAN_POINT('Ctrl Pts',(-5.99516084225658,2.25068705381848,-0.514353668096137));
#29595=CARTESIAN_POINT('Ctrl Pts',(-5.88413934517776,1.65446804044193,1.61024451971318));
#29596=CARTESIAN_POINT('Ctrl Pts',(-5.77311784809893,-0.453200896089194,
2.26379346626278));
#29597=CARTESIAN_POINT('Ctrl Pts',(-5.66209635102011,-2.14684523811403,
0.849239326513562));
#29598=CARTESIAN_POINT('Ctrl Pts',(-5.55107485394128,-1.87922530010751,
-1.34114286395817));
#29599=CARTESIAN_POINT('Ctrl Pts',(-5.44005335686246,0.105173001704038,
-2.30631536217895));
#29600=CARTESIAN_POINT('Ctrl Pts',(-5.32903185978363,1.99348983112823,-1.16453862250183));
#29601=CARTESIAN_POINT('Ctrl Pts',(-5.21801036270481,2.06064119925807,1.04110986837623));
#29602=CARTESIAN_POINT('Ctrl Pts',(-5.10698886562598,0.245280541688206,
2.29564574052253));
#29603=CARTESIAN_POINT('Ctrl Pts',(-4.99596736854716,-1.79415773287021,
1.45297967628323));
#29604=CARTESIAN_POINT('Ctrl Pts',(-4.88494587146833,-2.19453166699596,
-0.717065319662008));
#29605=CARTESIAN_POINT('Ctrl Pts',(-4.77392437438951,-0.590077077171925,
-2.23203067924847));
#29606=CARTESIAN_POINT('Ctrl Pts',(-4.66290287731068,1.55344622304472,-1.70791005097405));
#29607=CARTESIAN_POINT('Ctrl Pts',(-4.55188138023186,2.27780873136201,0.376482793021167));
#29608=CARTESIAN_POINT('Ctrl Pts',(-4.44085988315303,0.921264417775247,
2.11693735917044));
#29609=CARTESIAN_POINT('Ctrl Pts',(-4.3298383860742,-1.27690693206398,1.92345018052377));
#29610=CARTESIAN_POINT('Ctrl Pts',(-4.21881688899537,-2.30855173852655,
-0.0272172859738563));
#29611=CARTESIAN_POINT('Ctrl Pts',(-4.10779539191655,-1.23120425109033,
-1.95302022575508));
#29612=CARTESIAN_POINT('Ctrl Pts',(-3.99677389483772,0.970917801469463,
-2.09462897261033));
#29613=CARTESIAN_POINT('Ctrl Pts',(-3.88575239775891,2.28605164963331,-0.322675944744844));
#29614=CARTESIAN_POINT('Ctrl Pts',(-3.77473090068007,1.51274830487346,1.74405976853459));
#29615=CARTESIAN_POINT('Ctrl Pts',(-3.66370940360125,-0.642535986794508,
2.21749845902402));
#29616=CARTESIAN_POINT('Ctrl Pts',(-3.55268790652242,-2.21082739365792,
0.665127164948678));
#29617=CARTESIAN_POINT('Ctrl Pts',(-3.4416664094436,-1.75940321064622,-1.49487533009738));
#29618=CARTESIAN_POINT('Ctrl Pts',(-3.33064491236477,0.299335095435475,
-2.28922484930345));
#29619=CARTESIAN_POINT('Ctrl Pts',(-3.21962341528595,2.08461389911976,-0.992238278678359));
#29620=CARTESIAN_POINT('Ctrl Pts',(-3.10860191820712,1.96548026299592,1.21121395560337));
#29621=CARTESIAN_POINT('Ctrl Pts',(-2.99758042112829,0.050769486586585,
2.30815388756997));
#29622=CARTESIAN_POINT('Ctrl Pts',(-2.88655892404947,-1.91032208061755,
1.2964649854169));
#29623=CARTESIAN_POINT('Ctrl Pts',(-2.77553742697064,-2.12622662072629,
-0.8996178464995));
#29624=CARTESIAN_POINT('Ctrl Pts',(-2.66451592989181,-0.399703150196944,
-2.27384900489376));
#29625=CARTESIAN_POINT('Ctrl Pts',(-2.55349443281299,1.69197170262792,-1.5707907782725));
#29626=CARTESIAN_POINT('Ctrl Pts',(-2.44247293573417,2.23793492468817,0.567273476545088));
#29627=CARTESIAN_POINT('Ctrl Pts',(-2.33145143865534,0.739418289337298,
2.18710138509976));
#29628=CARTESIAN_POINT('Ctrl Pts',(-2.22042994157651,-1.43459866614401,
1.80888877426244));
#29629=CARTESIAN_POINT('Ctrl Pts',(-2.10940844449769,-2.29802880948203,
-0.221845857900401));
#29630=CARTESIAN_POINT('Ctrl Pts',(-1.99838694741886,-1.06207989233547,
-2.04991169691596));
#29631=CARTESIAN_POINT('Ctrl Pts',(-1.88736545034004,1.14413883704918,-2.00526767278129));
#29632=CARTESIAN_POINT('Ctrl Pts',(-1.77634395326121,2.30512237374665,-0.128698166199081));
#29633=CARTESIAN_POINT('Ctrl Pts',(-1.66532245618239,1.36024614796476,1.86544381076144));
#29634=CARTESIAN_POINT('Ctrl Pts',(-1.55430095910356,-0.827290961865428,
2.1553986720195));
#29635=CARTESIAN_POINT('Ctrl Pts',(-1.44327946202473,-2.25905249185057,
0.476273153560824));
#29636=CARTESIAN_POINT('Ctrl Pts',(-1.33225796494591,-1.62703941662637,
-1.63795085746574));
#29637=CARTESIAN_POINT('Ctrl Pts',(-1.22123646786708,0.491360911049524,
-2.25582176774822));
#29638=CARTESIAN_POINT('Ctrl Pts',(-1.11021497078826,2.16088497545151,-0.812858021785275));
#29639=CARTESIAN_POINT('Ctrl Pts',(-0.999193473709431,1.85630028593178,
1.37267043894513));
#29640=CARTESIAN_POINT('Ctrl Pts',(-0.888171976630606,-0.144084490198471,
2.30423829946203));
#29641=CARTESIAN_POINT('Ctrl Pts',(-0.777150479551781,-2.01290653192051,
1.13065678261724));
#29642=CARTESIAN_POINT('Ctrl Pts',(-0.666128982472955,-2.04269814678982,
-1.07565765858493));
#29643=CARTESIAN_POINT('Ctrl Pts',(-0.555107485394129,-0.206610916552875,
-2.2996518687847));
#29644=CARTESIAN_POINT('Ctrl Pts',(-0.444085988315305,1.81868635599406,
-1.42211079441787));
#29645=CARTESIAN_POINT('Ctrl Pts',(-0.333064491236478,2.18163438183212,
0.753324392930728));
#29646=CARTESIAN_POINT('Ctrl Pts',(-0.222042994157653,0.553226055458001,
2.24302138042127));
#29647=CARTESIAN_POINT('Ctrl Pts',(-0.111021497078828,-1.58398475473698,
1.67871039460253));
#29648=CARTESIAN_POINT('Ctrl Pts',(-0.0370071656929422,-2.03883201741979,
0.287355495504613));
#29649=CARTESIAN_POINT('Ctrl Pts',(0.,-1.92218901323832,-0.351148682734097));
#29650=CARTESIAN_POINT('Ctrl Pts',(-15.7993827215147,1.05793541951259,-1.48236995244726));
#29651=CARTESIAN_POINT('Ctrl Pts',(-15.7623755558218,1.55034246263605,-1.13094968055241));
#29652=CARTESIAN_POINT('Ctrl Pts',(-15.6883612244359,2.14904710443863,0.0949702857508803));
#29653=CARTESIAN_POINT('Ctrl Pts',(-15.5773397273571,1.08561464780462,1.85947873778831));
#29654=CARTESIAN_POINT('Ctrl Pts',(-15.4663182302782,-0.970482091465297,
1.91977702456333));
#29655=CARTESIAN_POINT('Ctrl Pts',(-15.3552967331994,-2.1395185329741,0.228996997483074));
#29656=CARTESIAN_POINT('Ctrl Pts',(-15.2442752361206,-1.35423117190993,
-1.6724127799477));
#29657=CARTESIAN_POINT('Ctrl Pts',(-15.1332537390418,0.668352646562777,
-2.04523047030762));
#29658=CARTESIAN_POINT('Ctrl Pts',(-15.0222322419629,2.08029037091456,-0.550007866879181));
#29659=CARTESIAN_POINT('Ctrl Pts',(-14.9112107448841,1.59180129537846,1.44788452227822));
#29660=CARTESIAN_POINT('Ctrl Pts',(-14.8001892478053,-0.350906933858996,
2.12294415771364));
#29661=CARTESIAN_POINT('Ctrl Pts',(-14.6891677507265,-1.97303197729494,
0.858631526263166));
#29662=CARTESIAN_POINT('Ctrl Pts',(-14.5781462536476,-1.7926861645986,-1.19011942496844));
#29663=CARTESIAN_POINT('Ctrl Pts',(-14.4671247565688,0.0253823607806043,
-2.15161337368581));
#29664=CARTESIAN_POINT('Ctrl Pts',(-14.35610325949,1.82026123117149,-1.14749535433649));
#29665=CARTESIAN_POINT('Ctrl Pts',(-14.2450817624112,1.9522294968358,0.90492877585299));
#29666=CARTESIAN_POINT('Ctrl Pts',(-14.1340602653323,0.300725548605529,
2.1306471165121));
#29667=CARTESIAN_POINT('Ctrl Pts',(-14.0230387682535,-1.62550795109711,
1.40990027548872));
#29668=CARTESIAN_POINT('Ctrl Pts',(-13.9120172711747,-2.06674831305342,
-0.598870664077681));
#29669=CARTESIAN_POINT('Ctrl Pts',(-13.8009957740958,-0.619897398695016,
-2.06053912400966));
#29670=CARTESIAN_POINT('Ctrl Pts',(-13.689974277017,1.39326474242623,-1.63978898384522));
#29671=CARTESIAN_POINT('Ctrl Pts',(-13.5789527799382,2.13360092975018,0.279001024356398));
#29672=CARTESIAN_POINT('Ctrl Pts',(-13.4679312828594,0.9247722518186,1.94290780360304));
#29673=CARTESIAN_POINT('Ctrl Pts',(-13.3569097857805,-1.12888806234094,
1.83185868350156));
#29674=CARTESIAN_POINT('Ctrl Pts',(-13.2458882887017,-2.15124542621297,
0.0473032636800278));
#29675=CARTESIAN_POINT('Ctrl Pts',(-13.1348667916229,-1.20831868869478,
-1.7804663500513));
#29676=CARTESIAN_POINT('Ctrl Pts',(-13.0238452945441,0.838475360538852,
-1.98167947787823));
#29677=CARTESIAN_POINT('Ctrl Pts',(-12.9128237974652,2.11927484975544,-0.372516566684666));
#29678=CARTESIAN_POINT('Ctrl Pts',(-12.8018023003864,1.46399716443733,1.576961249755));
#29679=CARTESIAN_POINT('Ctrl Pts',(-12.6907808033076,-0.528724549683909,
2.08579597088056));
#29680=CARTESIAN_POINT('Ctrl Pts',(-12.5797593062288,-2.03842654968845,
0.689138362566185));
#29681=CARTESIAN_POINT('Ctrl Pts',(-12.4687378091499,-1.68591086001068,
-1.33708603062395));
#29682=CARTESIAN_POINT('Ctrl Pts',(-12.3577163120711,0.206779542927678,
-2.1418068778343));
#29683=CARTESIAN_POINT('Ctrl Pts',(-12.2466948149923,1.91056516401672,-0.989866271423035));
#29684=CARTESIAN_POINT('Ctrl Pts',(-12.1356733179135,1.86894168698282,1.066373036002));
#29685=CARTESIAN_POINT('Ctrl Pts',(-12.0246518208346,0.119934507080401,
2.14842039537931));
#29686=CARTESIAN_POINT('Ctrl Pts',(-11.9136303237558,-1.73863961342216,
1.26776447966517));
#29687=CARTESIAN_POINT('Ctrl Pts',(-11.802608826677,-2.00886832871558,-0.771065833211139));
#29688=CARTESIAN_POINT('Ctrl Pts',(-11.6915873295982,-0.443882457299119,
-2.10548399313942));
#29689=CARTESIAN_POINT('Ctrl Pts',(-11.5805658325193,1.5266150889125,-1.51642370449935));
#29690=CARTESIAN_POINT('Ctrl Pts',(-11.4695443354405,2.10246359844209,0.45797521602046));
#29691=CARTESIAN_POINT('Ctrl Pts',(-11.3585228383617,0.757592960413117,
2.01398793134313));
#29692=CARTESIAN_POINT('Ctrl Pts',(-11.2475013412829,-1.27938160093674,
1.73010901403572));
#29693=CARTESIAN_POINT('Ctrl Pts',(-11.136479844204,-2.14756886923941,-0.134322124525075));
#29694=CARTESIAN_POINT('Ctrl Pts',(-11.0254583471252,-1.05383077964032,
-1.8760424220006));
#29695=CARTESIAN_POINT('Ctrl Pts',(-10.9144368500464,1.00264119902189,-1.9038920944442));
#29696=CARTESIAN_POINT('Ctrl Pts',(-10.8034153529675,2.14314385934751,-0.19242889441091));
#29697=CARTESIAN_POINT('Ctrl Pts',(-10.6923938558887,1.32576365802854,1.6948289601945));
#29698=CARTESIAN_POINT('Ctrl Pts',(-10.5813723588099,-0.702776463014917,
2.03376491372415));
#29699=CARTESIAN_POINT('Ctrl Pts',(-10.4703508617311,-2.0892906246237,0.51474184512501));
#29700=CARTESIAN_POINT('Ctrl Pts',(-10.3593293646523,-1.56711989366027,
-1.47452694792513));
#29701=CARTESIAN_POINT('Ctrl Pts',(-10.2483078675734,0.386703298969398,
-2.11673216062622));
#29702=CARTESIAN_POINT('Ctrl Pts',(-10.1372863704946,1.98725120478555,-0.8251830889818));
#29703=CARTESIAN_POINT('Ctrl Pts',(-10.0262648734158,1.77233298654189,1.22021730281073));
#29704=CARTESIAN_POINT('Ctrl Pts',(-9.91524337633695,-0.0617114347062867,
2.1508803267708));
#29705=CARTESIAN_POINT('Ctrl Pts',(-9.80422187925813,-1.83937897772859,
1.11659278949547));
#29706=CARTESIAN_POINT('Ctrl Pts',(-9.6932003821793,-1.93667002112544,-0.937765274755445));
#29707=CARTESIAN_POINT('Ctrl Pts',(-9.58217888510048,-0.264703706233324,
-2.13542183869359));
#29708=CARTESIAN_POINT('Ctrl Pts',(-9.47115738802165,1.64908438258572,-1.38225004263882));
#29709=CARTESIAN_POINT('Ctrl Pts',(-9.36013589094283,2.05634082352307,0.633685173233227));
#29710=CARTESIAN_POINT('Ctrl Pts',(-9.249114393864,0.585013874681943,2.07071322198242));
#29711=CARTESIAN_POINT('Ctrl Pts',(-9.13809289678517,-1.42075626334053,
1.61602788386891));
#29712=CARTESIAN_POINT('Ctrl Pts',(-9.02707139970635,-2.12858537587554,
-0.314990125038813));
#29713=CARTESIAN_POINT('Ctrl Pts',(-8.91604990262752,-0.891831623010708,
-1.95824687857819));
#29714=CARTESIAN_POINT('Ctrl Pts',(-8.8050284055487,1.15966064707945,-1.81253459687766));
#29715=CARTESIAN_POINT('Ctrl Pts',(-8.69400690846987,2.15173747180057,-0.0109696723941425));
#29716=CARTESIAN_POINT('Ctrl Pts',(-8.58298541139105,1.1780806849295,1.80061666688365));
#29717=CARTESIAN_POINT('Ctrl Pts',(-8.47196391431222,-0.871819291402609,
1.96723806500419));
#29718=CARTESIAN_POINT('Ctrl Pts',(-8.36094241723339,-2.12526314480885,
0.336676471676244));
#29719=CARTESIAN_POINT('Ctrl Pts',(-8.24992092015458,-1.43715917838138,
-1.60145807852011));
#29720=CARTESIAN_POINT('Ctrl Pts',(-8.13889942307573,0.563870802105082,
-2.07657029734043));
#29721=CARTESIAN_POINT('Ctrl Pts',(-8.02787792599693,2.04977298339684,-0.654618360420469));
#29722=CARTESIAN_POINT('Ctrl Pts',(-7.91685642891809,1.66309186751476,1.36536439146091));
#29723=CARTESIAN_POINT('Ctrl Pts',(-7.80583493183928,-0.242917524229776,
2.13800971880047));
#29724=CARTESIAN_POINT('Ctrl Pts',(-7.69481343476043,-1.92700804878851,
0.957462511625111));
#29725=CARTESIAN_POINT('Ctrl Pts',(-7.58379193768163,-1.85066797205159,
-1.09778073333686));
#29726=CARTESIAN_POINT('Ctrl Pts',(-7.47277044060278,-0.0836382622923028,
-2.15013932626328));
#29727=CARTESIAN_POINT('Ctrl Pts',(-7.36174894352397,1.75979972011074,-1.23822430373551));
#29728=CARTESIAN_POINT('Ctrl Pts',(-7.25072744644514,1.99556134569621,0.80487849817616));
#29729=CARTESIAN_POINT('Ctrl Pts',(-7.13970594936632,0.408265064525669,
2.11267936950949));
#29730=CARTESIAN_POINT('Ctrl Pts',(-7.02868445228748,-1.55200439311022,
1.49042840989756));
#29731=CARTESIAN_POINT('Ctrl Pts',(-6.91766295520867,-2.09443025186013,
-0.493413012957979));
#29732=CARTESIAN_POINT('Ctrl Pts',(-6.80664145812983,-0.723475878507756,
-2.02649380321791));
#29733=CARTESIAN_POINT('Ctrl Pts',(-6.69561996105102,1.30841453848234,-1.70825814113419));
#29734=CARTESIAN_POINT('Ctrl Pts',(-6.58459846397218,2.14499443553322,0.170567736675779));
#29735=CARTESIAN_POINT('Ctrl Pts',(-6.47357696689336,1.02200086515847,1.89357036121674));
#29736=CARTESIAN_POINT('Ctrl Pts',(-6.36255546981454,-1.03464817111157,
1.88668959908053));
#29737=CARTESIAN_POINT('Ctrl Pts',(-6.2515339727357,-2.14608771376038,0.156211414787358));
#29738=CARTESIAN_POINT('Ctrl Pts',(-6.14051247565689,-1.29695501762504,
-1.71697471254541));
#29739=CARTESIAN_POINT('Ctrl Pts',(-6.02949097857805,0.737019279440051,
-2.02160754425701));
#29740=CARTESIAN_POINT('Ctrl Pts',(-5.91846948149923,2.09768487180779,-0.479387796936746));
#29741=CARTESIAN_POINT('Ctrl Pts',(-5.8074479844204,1.54199695307992,1.500779756645));
#29742=CARTESIAN_POINT('Ctrl Pts',(-5.69642648734159,-0.42239220330661,
2.1099003075617));
#29743=CARTESIAN_POINT('Ctrl Pts',(-5.58540499026275,-2.00090224470079,
0.791507857455957));
#29744=CARTESIAN_POINT('Ctrl Pts',(-5.47438349318393,-1.7514751666901,-1.2499716883718));
#29745=CARTESIAN_POINT('Ctrl Pts',(-5.36336199610511,0.0980233188007598,
-2.14953155599876));
#29746=CARTESIAN_POINT('Ctrl Pts',(-5.25234049902627,1.85797197072144,-1.08537304060708));
#29747=CARTESIAN_POINT('Ctrl Pts',(-5.14131900194746,1.92055837464115,0.970334999296067));
#29748=CARTESIAN_POINT('Ctrl Pts',(-5.03029750486862,0.228606318579576,
2.1395872574795));
#29749=CARTESIAN_POINT('Ctrl Pts',(-4.91927600778981,-1.6721905106681,1.35420581053794));
#29750=CARTESIAN_POINT('Ctrl Pts',(-4.80825451071097,-2.04534694006012,
-0.668319067549202));
#29751=CARTESIAN_POINT('Ctrl Pts',(-4.69723301363215,-0.549963512645648,
-2.08029676152747));
#29752=CARTESIAN_POINT('Ctrl Pts',(-4.58621151655332,1.44784262019871,-1.59180596443137));
#29753=CARTESIAN_POINT('Ctrl Pts',(-4.4751900194745,2.12296281197481,0.350889413113472));
#29754=CARTESIAN_POINT('Ctrl Pts',(-4.36416852239567,0.858636667778067,
1.97302750969425));
#29755=CARTESIAN_POINT('Ctrl Pts',(-4.25314702531685,-1.19010252871572,
1.79269363038069));
#29756=CARTESIAN_POINT('Ctrl Pts',(-4.14212552823802,-2.15161590300918,
-0.0253670491160354));
#29757=CARTESIAN_POINT('Ctrl Pts',(-4.03110403115919,-1.14750672566223,
-1.82025349768217));
#29758=CARTESIAN_POINT('Ctrl Pts',(-3.92008253408037,0.904914603945486,
-1.95223565197143));
#29759=CARTESIAN_POINT('Ctrl Pts',(-3.80906103700155,2.13064537491839,-0.300740365764828));
#29760=CARTESIAN_POINT('Ctrl Pts',(-3.69803953992272,1.40991135511363,1.62549821654534));
#29761=CARTESIAN_POINT('Ctrl Pts',(-3.5870180428439,-0.598856254495366,
2.0667524447079));
#29762=CARTESIAN_POINT('Ctrl Pts',(-3.47599654576507,-2.06053487977653,
0.619911679579849));
#29763=CARTESIAN_POINT('Ctrl Pts',(-3.36497504868625,-1.63979860821658,
-1.39325338894354));
#29764=CARTESIAN_POINT('Ctrl Pts',(-3.25395355160741,0.278986232328857,
-2.13360285980372));
#29765=CARTESIAN_POINT('Ctrl Pts',(-3.1429320545286,1.94290140529526,-0.92478571060375));
#29766=CARTESIAN_POINT('Ctrl Pts',(-3.03191055744976,1.83186649895568,1.12887537469107));
#29767=CARTESIAN_POINT('Ctrl Pts',(-2.92088906037094,0.0473181661490567,
2.15124509804478));
#29768=CARTESIAN_POINT('Ctrl Pts',(-2.80986756329212,-1.78045798148312,
1.20833102146455));
#29769=CARTESIAN_POINT('Ctrl Pts',(-2.69884606621329,-1.98168528528455,
-0.838461634996595));
#29770=CARTESIAN_POINT('Ctrl Pts',(-2.58782456913446,-0.372531245496584,
-2.11927226854948));
#29771=CARTESIAN_POINT('Ctrl Pts',(-2.47680307205564,1.57695110837729,-1.46400808889317));
#29772=CARTESIAN_POINT('Ctrl Pts',(-2.36578157497681,2.08579963511323,0.528710105613121));
#29773=CARTESIAN_POINT('Ctrl Pts',(-2.25476007789799,0.689152477617587,
2.03842177029897));
#29774=CARTESIAN_POINT('Ctrl Pts',(-2.14373858081916,-1.33707434535616,
1.6859201327504));
#29775=CARTESIAN_POINT('Ctrl Pts',(-2.03271708374034,-2.14180832490704,
-0.206764729552862));
#29776=CARTESIAN_POINT('Ctrl Pts',(-1.92169558666151,-0.989879476590722,
-1.9105582661379));
#29777=CARTESIAN_POINT('Ctrl Pts',(-1.81067408958268,1.06636003688472,-1.86894915220754));
#29778=CARTESIAN_POINT('Ctrl Pts',(-1.69965259250385,2.14841966717244,-0.119949237637093));
#29779=CARTESIAN_POINT('Ctrl Pts',(-1.58863109542503,1.26777632709065,1.738630545905));
#29780=CARTESIAN_POINT('Ctrl Pts',(-1.4776095983462,-0.771051547279393,
2.00887421436004));
#29781=CARTESIAN_POINT('Ctrl Pts',(-1.36658810126738,-2.1054816255929,0.443896003834786));
#29782=CARTESIAN_POINT('Ctrl Pts',(-1.25556660418855,-1.51643293291336,
-1.52660261169636));
#29783=CARTESIAN_POINT('Ctrl Pts',(-1.14454510710973,0.457958092377877,
-2.10247052679843));
#29784=CARTESIAN_POINT('Ctrl Pts',(-1.0335236100309,2.01398755772421,-0.757599761518903));
#29785=CARTESIAN_POINT('Ctrl Pts',(-0.922502112952076,1.73010859982741,
1.27935601214206));
#29786=CARTESIAN_POINT('Ctrl Pts',(-0.811480615873251,-0.13428959607632,
2.1475956924447));
#29787=CARTESIAN_POINT('Ctrl Pts',(-0.700459118794427,-1.87606872008661,
1.05379449536493));
#29788=CARTESIAN_POINT('Ctrl Pts',(-0.589437621715599,-1.90383509467522,
-1.00253422341843));
#29789=CARTESIAN_POINT('Ctrl Pts',(-0.478416124636775,-0.192565462740806,
-2.14332104829499));
#29790=CARTESIAN_POINT('Ctrl Pts',(-0.367394627557949,1.6950516728034,-1.32543540179154));
#29791=CARTESIAN_POINT('Ctrl Pts',(-0.256373130479123,2.03332641506991,
0.70211324134716));
#29792=CARTESIAN_POINT('Ctrl Pts',(-0.145351633400297,0.515617631183002,
2.09054031250966));
#29793=CARTESIAN_POINT('Ctrl Pts',(-0.0343301363214737,-1.47630513604666,
1.56459130687665));
#29794=CARTESIAN_POINT('Ctrl Pts',(0.0396841950644127,-1.90023178559759,
0.267821008135351));
#29795=CARTESIAN_POINT('Ctrl Pts',(0.0766913607573549,-1.79151819751408,
-0.32727752100269));
#29796=CARTESIAN_POINT('Ctrl Pts',(-15.7226913607574,0.98077109908141,-1.37424797458504));
#29797=CARTESIAN_POINT('Ctrl Pts',(-15.6856841950644,1.43726266555351,-1.04845980269021));
#29798=CARTESIAN_POINT('Ctrl Pts',(-15.6116698636785,1.99229863347336,0.0880432867810469));
#29799=CARTESIAN_POINT('Ctrl Pts',(-15.5006483665997,1.00643144342095,1.72385097591248));
#29800=CARTESIAN_POINT('Ctrl Pts',(-15.3896268695209,-0.899696493689348,
1.77975119052132));
#29801=CARTESIAN_POINT('Ctrl Pts',(-15.2786053724421,-1.98346506259976,
0.212294278805113));
#29802=CARTESIAN_POINT('Ctrl Pts',(-15.1675838753632,-1.25545545634186,
-1.55042934573719));
#29803=CARTESIAN_POINT('Ctrl Pts',(-15.0565623782844,0.619603945243983,
-1.89605423851159));
#29804=CARTESIAN_POINT('Ctrl Pts',(-14.9455408812056,1.92855691931587,-0.509891067217538));
#29805=CARTESIAN_POINT('Ctrl Pts',(-14.8345193841267,1.47569754938993,1.34227786315351));
#29806=CARTESIAN_POINT('Ctrl Pts',(-14.7234978870479,-0.325312276012785,
1.968099598942));
#29807=CARTESIAN_POINT('Ctrl Pts',(-14.6124763899691,-1.82912180195825,
0.796004151280846));
#29808=CARTESIAN_POINT('Ctrl Pts',(-14.5014548928903,-1.66193015899916,
-1.1033137892313));
#29809=CARTESIAN_POINT('Ctrl Pts',(-14.3904333958114,0.023531007111521,
-1.99467772265372));
#29810=CARTESIAN_POINT('Ctrl Pts',(-14.2794118987326,1.68749393902876,-1.06379865831688));
#29811=CARTESIAN_POINT('Ctrl Pts',(-14.1683904016538,1.80983662514383,0.83892454465003));
#29812=CARTESIAN_POINT('Ctrl Pts',(-14.057368904575,0.278791050368257,1.97524071476778));
#29813=CARTESIAN_POINT('Ctrl Pts',(-13.9463474074961,-1.50694568908335,
1.30706413386114));
#29814=CARTESIAN_POINT('Ctrl Pts',(-13.8353259104173,-1.91600260009437,
-0.555189880763887));
#29815=CARTESIAN_POINT('Ctrl Pts',(-13.7243044133385,-0.574682954953825,
-1.91024630055989));
#29816=CARTESIAN_POINT('Ctrl Pts',(-13.6132829162597,1.29164197316535,-1.52018508340368));
#29817=CARTESIAN_POINT('Ctrl Pts',(-13.5022614191808,1.97797908102583,0.25865108234011));
#29818=CARTESIAN_POINT('Ctrl Pts',(-13.391239922102,0.857320665408837,1.80119484309498));
#29819=CARTESIAN_POINT('Ctrl Pts',(-13.2802184250232,-1.04654855600932,
1.69824548950954));
#29820=CARTESIAN_POINT('Ctrl Pts',(-13.1691969279444,-1.99433661275166,
0.0438530302076145));
#29821=CARTESIAN_POINT('Ctrl Pts',(-13.0581754308656,-1.1201856242773,-1.65060164052528));
#29822=CARTESIAN_POINT('Ctrl Pts',(-12.9471539337867,0.777318147914217,
-1.83713856602054));
#29823=CARTESIAN_POINT('Ctrl Pts',(-12.8361324367079,1.96469792514163,-0.345345732636185));
#29824=CARTESIAN_POINT('Ctrl Pts',(-12.725110939629,1.35721527187243,1.46193991580655));
#29825=CARTESIAN_POINT('Ctrl Pts',(-12.6140894425503,-0.490160125221753,
1.93366094856961));
#29826=CARTESIAN_POINT('Ctrl Pts',(-12.5030679454714,-1.88974658628572,
0.638873580378455));
#29827=CARTESIAN_POINT('Ctrl Pts',(-12.3920464483926,-1.56294289483922,
-1.23956085752912));
#29828=CARTESIAN_POINT('Ctrl Pts',(-12.2810249513137,0.19169733411343,-1.98558649880676));
#29829=CARTESIAN_POINT('Ctrl Pts',(-12.170003454235,1.77121123011709,-0.917666818844631));
#29830=CARTESIAN_POINT('Ctrl Pts',(-12.0589819571561,1.73262371091205,0.988593287700225));
#29831=CARTESIAN_POINT('Ctrl Pts',(-11.9479604600773,0.111186652944486,
1.99171763569072));
#29832=CARTESIAN_POINT('Ctrl Pts',(-11.8369389629984,-1.61182568719379,
1.17529552292561));
#29833=CARTESIAN_POINT('Ctrl Pts',(-11.7259174659196,-1.86234430034674,
-0.71482537662935));
#29834=CARTESIAN_POINT('Ctrl Pts',(-11.6148959688408,-0.41150629563833,
-1.95191295419624));
#29835=CARTESIAN_POINT('Ctrl Pts',(-11.503874471762,1.41526593307254,-1.40581789389388));
#29836=CARTESIAN_POINT('Ctrl Pts',(-11.3928529746831,1.94911286283686,0.424571148374424));
#29837=CARTESIAN_POINT('Ctrl Pts',(-11.2818314776043,0.702335196209829,
1.8670904863646));
#29838=CARTESIAN_POINT('Ctrl Pts',(-11.1708099805255,-1.186065307723,1.60391729771957));
#29839=CARTESIAN_POINT('Ctrl Pts',(-11.0597884834467,-1.99092821866891,
-0.124524857823653));
#29840=CARTESIAN_POINT('Ctrl Pts',(-10.9487669863679,-0.976965845864036,
-1.73920652831208));
#29841=CARTESIAN_POINT('Ctrl Pts',(-10.837745489289,0.929509961205432,-1.76502488484668));
#29842=CARTESIAN_POINT('Ctrl Pts',(-10.7267239922102,1.98682596277023,-0.1783934017006));
#29843=CARTESIAN_POINT('Ctrl Pts',(-10.6157024951314,1.22906432285431,1.57121052134806));
#29844=CARTESIAN_POINT('Ctrl Pts',(-10.5046809980525,-0.651516936976405,
1.88542496348729));
#29845=CARTESIAN_POINT('Ctrl Pts',(-10.3936595009737,-1.93690070718752,
0.477197299452391));
#29846=CARTESIAN_POINT('Ctrl Pts',(-10.2826380038949,-1.45281637437343,
-1.36697702777355));
#29847=CARTESIAN_POINT('Ctrl Pts',(-10.1716165068161,0.358497704636228,
-1.9623406961786));
#29848=CARTESIAN_POINT('Ctrl Pts',(-10.0605950097373,1.84230389900958,-0.76499539593535));
#29849=CARTESIAN_POINT('Ctrl Pts',(-9.94957351265842,1.64306151310234,1.13121637022721));
#29850=CARTESIAN_POINT('Ctrl Pts',(-9.8385520155796,-0.0572102895190575,
1.99399814314891));
#29851=CARTESIAN_POINT('Ctrl Pts',(-9.72753051850077,-1.70521726406064,
1.03515008305931));
#29852=CARTESIAN_POINT('Ctrl Pts',(-9.61650902142195,-1.79541203569147,
-0.869365995540654));
#29853=CARTESIAN_POINT('Ctrl Pts',(-9.50548752434313,-0.245396590477122,
-1.97966717543389));
#29854=CARTESIAN_POINT('Ctrl Pts',(-9.39446602726429,1.52880248884355,-1.28143067007698));
#29855=CARTESIAN_POINT('Ctrl Pts',(-9.28344453018548,1.90635421820158,0.587465068623835));
#29856=CARTESIAN_POINT('Ctrl Pts',(-9.17242303310664,0.542343786082916,
1.91967831414678));
#29857=CARTESIAN_POINT('Ctrl Pts',(-9.06140153602782,-1.3171283012391,1.49815708461536));
#29858=CARTESIAN_POINT('Ctrl Pts',(-8.95038003894899,-1.9733293545913,-0.292015188674224));
#29859=CARTESIAN_POINT('Ctrl Pts',(-8.83935854187017,-0.82678267970151,
-1.81541510753154));
#29860=CARTESIAN_POINT('Ctrl Pts',(-8.72833704479135,1.0750766317301,-1.6803308745649));
#29861=CARTESIAN_POINT('Ctrl Pts',(-8.61731554771252,1.99479276922667,-0.0101695599297692));
#29862=CARTESIAN_POINT('Ctrl Pts',(-8.50629405063369,1.09215313794598,1.6692822216099));
#29863=CARTESIAN_POINT('Ctrl Pts',(-8.39527255355487,-0.808230019393109,
1.82375048947492));
#29864=CARTESIAN_POINT('Ctrl Pts',(-8.28425105647603,-1.97024944238251,
0.312119763711931));
#29865=CARTESIAN_POINT('Ctrl Pts',(-8.17322955939722,-1.33233481074433,
-1.48464998036137));
#29866=CARTESIAN_POINT('Ctrl Pts',(-8.06220806231839,0.52274285946047,-1.92510818267215));
#29867=CARTESIAN_POINT('Ctrl Pts',(-7.95118656523957,1.90026542708978,-0.606871418601563));
#29868=CARTESIAN_POINT('Ctrl Pts',(-7.84016506816073,1.54178828753771,1.26577663452906));
#29869=CARTESIAN_POINT('Ctrl Pts',(-7.72914357108192,-0.225199461924381,
1.98206629920827));
#29870=CARTESIAN_POINT('Ctrl Pts',(-7.61812207400307,-1.78645479401735,
0.88762654367734));
#29871=CARTESIAN_POINT('Ctrl Pts',(-7.50710057692427,-1.71568285502723,
-1.01771015179853));
#29872=CARTESIAN_POINT('Ctrl Pts',(-7.39607907984543,-0.0775378051634432,
-1.99331119017544));
#29873=CARTESIAN_POINT('Ctrl Pts',(-7.28505758276661,1.63144240548383,-1.14790996584979));
#29874=CARTESIAN_POINT('Ctrl Pts',(-7.17403608568779,1.85000790993892,0.746171793403911));
#29875=CARTESIAN_POINT('Ctrl Pts',(-7.06301458860896,0.378486785361485,
1.95858350994154));
#29876=CARTESIAN_POINT('Ctrl Pts',(-6.95199309153013,-1.4388033771581,1.38171865949137));
#29877=CARTESIAN_POINT('Ctrl Pts',(-6.8409715944513,-1.94166545724747,-0.457424162282821));
#29878=CARTESIAN_POINT('Ctrl Pts',(-6.72995009737248,-0.670706566238076,
-1.87868419754713));
#29879=CARTESIAN_POINT('Ctrl Pts',(-6.61892860029366,1.21298062366854,-1.58366019673188));
#29880=CARTESIAN_POINT('Ctrl Pts',(-6.50790710321483,1.98854156053368,0.158126766040605));
#29881=CARTESIAN_POINT('Ctrl Pts',(-6.396885606136,0.947457560543175,1.75545600431277));
#29882=CARTESIAN_POINT('Ctrl Pts',(-6.28586410905718,-0.95918238980143,
1.74907711528194));
#29883=CARTESIAN_POINT('Ctrl Pts',(-6.17484261197835,-1.98955509658577,
0.144817574063867));
#29884=CARTESIAN_POINT('Ctrl Pts',(-6.06382111489954,-1.20235694413303,
-1.59174099369315));
#29885=CARTESIAN_POINT('Ctrl Pts',(-5.9527996178207,0.683262130569029,-1.87415433543731));
#29886=CARTESIAN_POINT('Ctrl Pts',(-5.84177812074188,1.9446826897971,-0.444421925777357));
#29887=CARTESIAN_POINT('Ctrl Pts',(-5.73075662366305,1.4295258657179,1.39131499357682));
#29888=CARTESIAN_POINT('Ctrl Pts',(-5.61973512658423,-0.391583510524026,
1.95600714886062));
#29889=CARTESIAN_POINT('Ctrl Pts',(-5.50871362950539,-1.85495925128755,
0.73377638839835));
#29890=CARTESIAN_POINT('Ctrl Pts',(-5.39769213242658,-1.62372503327269,
-1.15880051278543));
#29891=CARTESIAN_POINT('Ctrl Pts',(-5.28667063534774,0.09087363589748,-1.99274774981856));
#29892=CARTESIAN_POINT('Ctrl Pts',(-5.17564913826893,1.72245411031465,-1.00620745871233));
#29893=CARTESIAN_POINT('Ctrl Pts',(-5.0646276411901,1.78047555002424,0.899560130215906));
#29894=CARTESIAN_POINT('Ctrl Pts',(-4.95360614411127,0.211932095470946,
1.98352877443648));
#29895=CARTESIAN_POINT('Ctrl Pts',(-4.84258464703245,-1.55022328846599,
1.25543194479265));
#29896=CARTESIAN_POINT('Ctrl Pts',(-4.73156314995362,-1.89616221312428,
-0.619572815436396));
#29897=CARTESIAN_POINT('Ctrl Pts',(-4.6205416528748,-0.509849948119368,
-1.92856284380646));
#29898=CARTESIAN_POINT('Ctrl Pts',(-4.50952015579597,1.3422390173527,-1.4757018778887));
#29899=CARTESIAN_POINT('Ctrl Pts',(-4.39849865871714,1.96811689258761,0.325296033205782));
#29900=CARTESIAN_POINT('Ctrl Pts',(-4.28747716163832,0.796008917780889,
1.82911766021806));
#29901=CARTESIAN_POINT('Ctrl Pts',(-4.17645566455949,-1.10329812536747,
1.66193708023761));
#29902=CARTESIAN_POINT('Ctrl Pts',(-4.06543416748067,-1.9946800674918,-0.0235168122582161));
#29903=CARTESIAN_POINT('Ctrl Pts',(-3.95441267040184,-1.06380920023413,
-1.68748676960926));
#29904=CARTESIAN_POINT('Ctrl Pts',(-3.84339117332301,0.838911406421511,
-1.80984233133253));
#29905=CARTESIAN_POINT('Ctrl Pts',(-3.73236967624419,1.97523910020347,-0.27880478678481));
#29906=CARTESIAN_POINT('Ctrl Pts',(-3.62134817916536,1.30707440535381,1.50693666455608));
#29907=CARTESIAN_POINT('Ctrl Pts',(-3.51032668208654,-0.555176522196224,
1.91600643039178));
#29908=CARTESIAN_POINT('Ctrl Pts',(-3.39930518500771,-1.91024236589515,
0.574696194211018));
#29909=CARTESIAN_POINT('Ctrl Pts',(-3.28828368792889,-1.52019400578695,
-1.29163144778971));
#29910=CARTESIAN_POINT('Ctrl Pts',(-3.17726219085006,0.258637369222239,
-1.97798087030399));
#29911=CARTESIAN_POINT('Ctrl Pts',(-3.06624069377124,1.80118891147076,-0.857333142529141));
#29912=CARTESIAN_POINT('Ctrl Pts',(-2.95521919669241,1.69825273491544,1.04653679377876));
#29913=CARTESIAN_POINT('Ctrl Pts',(-2.84419769961359,0.0438668457115283,
1.9943363085196));
#29914=CARTESIAN_POINT('Ctrl Pts',(-2.73317620253476,-1.65059388234868,
1.1201970575122));
#29915=CARTESIAN_POINT('Ctrl Pts',(-2.62215470545594,-1.83714394984282,
-0.777305423493693));
#29916=CARTESIAN_POINT('Ctrl Pts',(-2.51113320837711,-0.345359340796222,
-1.9646955322052));
#29917=CARTESIAN_POINT('Ctrl Pts',(-2.40011171129828,1.46193051412666,-1.35722539951385));
#29918=CARTESIAN_POINT('Ctrl Pts',(-2.28909021421946,1.9336643455383,0.490146734681156));
#29919=CARTESIAN_POINT('Ctrl Pts',(-2.17806871714063,0.638886665897876,
1.88974215549818));
#29920=CARTESIAN_POINT('Ctrl Pts',(-2.06704722006181,-1.23955002456831,
1.56295149123835));
#29921=CARTESIAN_POINT('Ctrl Pts',(-1.95602572298298,-1.98558784033205,
-0.191683601205323));
#29922=CARTESIAN_POINT('Ctrl Pts',(-1.84500422590415,-0.917679060845975,
-1.77120483535984));
#29923=CARTESIAN_POINT('Ctrl Pts',(-1.73398272882533,0.988581236720258,
-1.73263063163378));
#29924=CARTESIAN_POINT('Ctrl Pts',(-1.6229612317465,1.99171696059823,-0.111200309075107));
#29925=CARTESIAN_POINT('Ctrl Pts',(-1.51193973466768,1.17530650621655,1.61181728104857));
#29926=CARTESIAN_POINT('Ctrl Pts',(-1.40091823758885,-0.714812132693357,
1.86234975670057));
#29927=CARTESIAN_POINT('Ctrl Pts',(-1.28989674051002,-1.95191075933523,
0.411518854108752));
#29928=CARTESIAN_POINT('Ctrl Pts',(-1.1788752434312,-1.40582644920036,-1.41525436592699));
#29929=CARTESIAN_POINT('Ctrl Pts',(-1.06785374635237,0.42455527370623,-1.94911928584864));
#29930=CARTESIAN_POINT('Ctrl Pts',(-0.956832249273549,1.86709013999691,
-0.702341501252534));
#29931=CARTESIAN_POINT('Ctrl Pts',(-0.845810752194721,1.60391691372304,
1.18604158533899));
#29932=CARTESIAN_POINT('Ctrl Pts',(-0.734789255115897,-0.124494701954168,
1.99095308542736));
#29933=CARTESIAN_POINT('Ctrl Pts',(-0.623767758037071,-1.73923090825272,
0.976932208112631));
#29934=CARTESIAN_POINT('Ctrl Pts',(-0.512746260958245,-1.76497204256062,
-0.929410788251921));
#29935=CARTESIAN_POINT('Ctrl Pts',(-0.40172476387942,-0.178520008928735,
-1.98699022780528));
#29936=CARTESIAN_POINT('Ctrl Pts',(-0.290703266800595,1.57141698961275,
-1.22876000916521));
#29937=CARTESIAN_POINT('Ctrl Pts',(-0.179681769721768,1.88501844830769,
0.650902089763596));
#29938=CARTESIAN_POINT('Ctrl Pts',(-0.0686602726429429,0.478009206908001,
1.93805924459805));
#29939=CARTESIAN_POINT('Ctrl Pts',(0.0423612244358815,-1.36862551735633,
1.45047221915076));
#29940=CARTESIAN_POINT('Ctrl Pts',(0.116375555821768,-1.76163155377538,
0.248286520766087));
#29941=CARTESIAN_POINT('Ctrl Pts',(0.15338272151471,-1.66084738178985,-0.303406359271283));
#29942=CARTESIAN_POINT('Ctrl Pts',(-15.646,0.903606778650232,-1.26612599672282));
#29943=CARTESIAN_POINT('Ctrl Pts',(-15.6089928343071,1.32418286847098,-0.965969924828001));
#29944=CARTESIAN_POINT('Ctrl Pts',(-15.5349785029212,1.83555016250808,0.0811162878112121));
#29945=CARTESIAN_POINT('Ctrl Pts',(-15.4239570058423,0.927248239037281,
1.58822321403664));
#29946=CARTESIAN_POINT('Ctrl Pts',(-15.3129355087635,-0.828910895913401,
1.63972535647931));
#29947=CARTESIAN_POINT('Ctrl Pts',(-15.2019140116847,-1.82741159222543,
0.195591560127152));
#29948=CARTESIAN_POINT('Ctrl Pts',(-15.0908925146059,-1.15667974077379,
-1.42844591152668));
#29949=CARTESIAN_POINT('Ctrl Pts',(-14.979871017527,0.570855243925188,-1.74687800671557));
#29950=CARTESIAN_POINT('Ctrl Pts',(-14.8688495204482,1.77682346771718,-0.469774267555894));
#29951=CARTESIAN_POINT('Ctrl Pts',(-14.7578280233694,1.3595938034014,1.2366712040288));
#29952=CARTESIAN_POINT('Ctrl Pts',(-14.6468065262906,-0.299717618166574,
1.81325504017035));
#29953=CARTESIAN_POINT('Ctrl Pts',(-14.5357850292117,-1.68521162662156,
0.733376776298527));
#29954=CARTESIAN_POINT('Ctrl Pts',(-14.4247635321329,-1.53117415339972,
-1.01650815349415));
#29955=CARTESIAN_POINT('Ctrl Pts',(-14.3137420350541,0.0216796534424384,
-1.83774207162163));
#29956=CARTESIAN_POINT('Ctrl Pts',(-14.2027205379753,1.55472664688603,-0.980101962297276));
#29957=CARTESIAN_POINT('Ctrl Pts',(-14.0916990408964,1.66744375345186,0.772920313447068));
#29958=CARTESIAN_POINT('Ctrl Pts',(-13.9806775438176,0.256856552130983,
1.81983431302347));
#29959=CARTESIAN_POINT('Ctrl Pts',(-13.8696560467388,-1.38838342706959,
1.20422799223356));
#29960=CARTESIAN_POINT('Ctrl Pts',(-13.75863454966,-1.76525688713531,-0.511509097450093));
#29961=CARTESIAN_POINT('Ctrl Pts',(-13.6476130525811,-0.529468511212632,
-1.75995347711011));
#29962=CARTESIAN_POINT('Ctrl Pts',(-13.5365915555023,1.19001920390447,-1.40058118296215));
#29963=CARTESIAN_POINT('Ctrl Pts',(-13.4255700584235,1.82235723230149,0.238301140323824));
#29964=CARTESIAN_POINT('Ctrl Pts',(-13.3145485613446,0.789869078999073,
1.65948188258691));
#29965=CARTESIAN_POINT('Ctrl Pts',(-13.2035270642659,-0.964209049677692,
1.56463229551752));
#29966=CARTESIAN_POINT('Ctrl Pts',(-13.092505567187,-1.83742779929035,0.0404027967352005));
#29967=CARTESIAN_POINT('Ctrl Pts',(-12.9814840701082,-1.03205255985982,
-1.52073693099926));
#29968=CARTESIAN_POINT('Ctrl Pts',(-12.8704625730293,0.716160935289581,
-1.69259765416285));
#29969=CARTESIAN_POINT('Ctrl Pts',(-12.7594410759505,1.81012100052783,-0.318174898587703));
#29970=CARTESIAN_POINT('Ctrl Pts',(-12.6484195788717,1.25043337930754,1.3469185818581));
#29971=CARTESIAN_POINT('Ctrl Pts',(-12.5373980817929,-0.451595700759593,
1.78152592625865));
#29972=CARTESIAN_POINT('Ctrl Pts',(-12.426376584714,-1.74106662288298,0.588608798190727));
#29973=CARTESIAN_POINT('Ctrl Pts',(-12.3153550876353,-1.43997492966776,
-1.14203568443429));
#29974=CARTESIAN_POINT('Ctrl Pts',(-12.2043335905564,0.176615125299183,
-1.82936611977922));
#29975=CARTESIAN_POINT('Ctrl Pts',(-12.0933120934776,1.63185729621746,-0.845467366266227));
#29976=CARTESIAN_POINT('Ctrl Pts',(-11.9822905963988,1.59630573484127,0.910813539398446));
#29977=CARTESIAN_POINT('Ctrl Pts',(-11.8712690993199,0.10243879880857,1.83501487600212));
#29978=CARTESIAN_POINT('Ctrl Pts',(-11.7602476022411,-1.48501176096542,
1.08282656618605));
#29979=CARTESIAN_POINT('Ctrl Pts',(-11.6492261051623,-1.7158202719779,-0.658584920047561));
#29980=CARTESIAN_POINT('Ctrl Pts',(-11.5382046080835,-0.379130133977537,
-1.79834191525306));
#29981=CARTESIAN_POINT('Ctrl Pts',(-11.4271831110046,1.30391677723258,-1.2952120832884));
#29982=CARTESIAN_POINT('Ctrl Pts',(-11.3161616139258,1.79576212723163,0.391167080728389));
#29983=CARTESIAN_POINT('Ctrl Pts',(-11.205140116847,0.647077432006542,1.72019304138606));
#29984=CARTESIAN_POINT('Ctrl Pts',(-11.0941186197681,-1.09274901450927,
1.47772558140343));
#29985=CARTESIAN_POINT('Ctrl Pts',(-10.9830971226893,-1.83428756809842,
-0.114727591122236));
#29986=CARTESIAN_POINT('Ctrl Pts',(-10.8720756256105,-0.900100912087758,
-1.60237063462356));
#29987=CARTESIAN_POINT('Ctrl Pts',(-10.7610541285317,0.85637872338898,-1.62615767524916));
#29988=CARTESIAN_POINT('Ctrl Pts',(-10.6500326314529,1.83050806619295,-0.164357908990289));
#29989=CARTESIAN_POINT('Ctrl Pts',(-10.539011134374,1.13236498768008,1.44759208250163));
#29990=CARTESIAN_POINT('Ctrl Pts',(-10.4279896372952,-0.600257410937894,
1.73708501325043));
#29991=CARTESIAN_POINT('Ctrl Pts',(-10.3169681402164,-1.78451078975135,
0.439652753779773));
#29992=CARTESIAN_POINT('Ctrl Pts',(-10.2059466431376,-1.33851285508659,
-1.25942710762198));
#29993=CARTESIAN_POINT('Ctrl Pts',(-10.0949251460587,0.330292110303061,
-1.80794923173099));
#29994=CARTESIAN_POINT('Ctrl Pts',(-9.98390364897991,1.69735659323361,-0.704807702888898));
#29995=CARTESIAN_POINT('Ctrl Pts',(-9.87288215190106,1.51379003966279,1.04221543764369));
#29996=CARTESIAN_POINT('Ctrl Pts',(-9.76186065482225,-0.0527091443318308,
1.83711595952703));
#29997=CARTESIAN_POINT('Ctrl Pts',(-9.65083915774341,-1.5710555503927,0.953707376623146));
#29998=CARTESIAN_POINT('Ctrl Pts',(-9.53981766066459,-1.6541540502575,-0.800966716325862));
#29999=CARTESIAN_POINT('Ctrl Pts',(-9.42879616358577,-0.226089474720918,
-1.82391251217418));
#30000=CARTESIAN_POINT('Ctrl Pts',(-9.31777466650694,1.40852059510137,-1.18061129751514));
#30001=CARTESIAN_POINT('Ctrl Pts',(-9.20675316942812,1.75636761288009,0.541244964014445));
#30002=CARTESIAN_POINT('Ctrl Pts',(-9.09573167234929,0.499673697483888,
1.76864340631115));
#30003=CARTESIAN_POINT('Ctrl Pts',(-8.98471017527046,-1.21350033913767,
1.38028628536181));
#30004=CARTESIAN_POINT('Ctrl Pts',(-8.87368867819165,-1.81807333330707,
-0.269040252309636));
#30005=CARTESIAN_POINT('Ctrl Pts',(-8.7626671811128,-0.761733736392313,
-1.67258333648488));
#30006=CARTESIAN_POINT('Ctrl Pts',(-8.651645684034,0.990492616380764,-1.54812715225214));
#30007=CARTESIAN_POINT('Ctrl Pts',(-8.54062418695516,1.83784806665277,-0.00936944746539623));
#30008=CARTESIAN_POINT('Ctrl Pts',(-8.42960268987634,1.00622559096247,1.53794777633616));
#30009=CARTESIAN_POINT('Ctrl Pts',(-8.31858119279751,-0.744640747383609,
1.68026291394564));
#30010=CARTESIAN_POINT('Ctrl Pts',(-8.20755969571868,-1.81523573995617,
0.287563055747619));
#30011=CARTESIAN_POINT('Ctrl Pts',(-8.09653819863986,-1.22751044310728,
-1.36784188220264));
#30012=CARTESIAN_POINT('Ctrl Pts',(-7.98551670156104,0.481614916815858,
-1.77364606800387));
#30013=CARTESIAN_POINT('Ctrl Pts',(-7.87449520448221,1.75075787078272,-0.559124476782657));
#30014=CARTESIAN_POINT('Ctrl Pts',(-7.76347370740338,1.42048470756065,1.16618887759722));
#30015=CARTESIAN_POINT('Ctrl Pts',(-7.65245221032457,-0.207481399618984,
1.82612287961606));
#30016=CARTESIAN_POINT('Ctrl Pts',(-7.54143071324572,-1.6459015392462,0.817790575729572));
#30017=CARTESIAN_POINT('Ctrl Pts',(-7.43040921616691,-1.58069773800288,
-0.937639570260189));
#30018=CARTESIAN_POINT('Ctrl Pts',(-7.31938771908807,-0.0714373480345857,
-1.8364830540876));
#30019=CARTESIAN_POINT('Ctrl Pts',(-7.20836622200926,1.50308509085693,-1.05759562796407));
#30020=CARTESIAN_POINT('Ctrl Pts',(-7.09734472493043,1.70445447418163,0.687465088631667));
#30021=CARTESIAN_POINT('Ctrl Pts',(-6.9863232278516,0.348708506197304,1.80448765037358));
#30022=CARTESIAN_POINT('Ctrl Pts',(-6.87530173077278,-1.32560236120598,
1.27300890908518));
#30023=CARTESIAN_POINT('Ctrl Pts',(-6.76428023369395,-1.78890066263481,
-0.421435311607665));
#30024=CARTESIAN_POINT('Ctrl Pts',(-6.65325873661513,-0.617937253968403,
-1.73087459187634));
#30025=CARTESIAN_POINT('Ctrl Pts',(-6.5422372395363,1.11754670885474,-1.45906225232958));
#30026=CARTESIAN_POINT('Ctrl Pts',(-6.43121574245748,1.83208868553414,0.145685795405434));
#30027=CARTESIAN_POINT('Ctrl Pts',(-6.32019424537864,0.872914255927876,
1.6173416474088));
#30028=CARTESIAN_POINT('Ctrl Pts',(-6.20917274829983,-0.883716608491293,
1.61146463148335));
#30029=CARTESIAN_POINT('Ctrl Pts',(-6.09815125122099,-1.83302247941115,
0.133423733340373));
#30030=CARTESIAN_POINT('Ctrl Pts',(-5.98712975414218,-1.10775887064102,
-1.46650727484089));
#30031=CARTESIAN_POINT('Ctrl Pts',(-5.87610825706334,0.629504981698008,
-1.72670112661761));
#30032=CARTESIAN_POINT('Ctrl Pts',(-5.76508675998453,1.79168050778642,-0.409456054617966));
#30033=CARTESIAN_POINT('Ctrl Pts',(-5.65406526290569,1.31705477835589,1.28185023050864));
#30034=CARTESIAN_POINT('Ctrl Pts',(-5.54304376582688,-0.360774817741443,
1.80211399015954));
#30035=CARTESIAN_POINT('Ctrl Pts',(-5.43202226874804,-1.7090162578743,0.676044919340745));
#30036=CARTESIAN_POINT('Ctrl Pts',(-5.32100077166922,-1.49597489985528,
-1.06762933719906));
#30037=CARTESIAN_POINT('Ctrl Pts',(-5.20997927459039,0.0837239529942017,
-1.83596394363836));
#30038=CARTESIAN_POINT('Ctrl Pts',(-5.09895777751157,1.58693624990787,-0.927041876817589));
#30039=CARTESIAN_POINT('Ctrl Pts',(-4.98793628043274,1.64039272540732,0.828785261135749));
#30040=CARTESIAN_POINT('Ctrl Pts',(-4.87691478335392,0.195257872362318,
1.82747029139345));
#30041=CARTESIAN_POINT('Ctrl Pts',(-4.76589328627509,-1.42825606626389,
1.15665807904736));
#30042=CARTESIAN_POINT('Ctrl Pts',(-4.65487178919627,-1.74697748618844,
-0.57082656332359));
#30043=CARTESIAN_POINT('Ctrl Pts',(-4.54385029211744,-0.469736383593091,
-1.77682892608546));
#30044=CARTESIAN_POINT('Ctrl Pts',(-4.43282879503861,1.2366354145067,-1.35959779134602));
#30045=CARTESIAN_POINT('Ctrl Pts',(-4.32180729795979,1.8132709732004,0.299702653298089));
#30046=CARTESIAN_POINT('Ctrl Pts',(-4.21078580088097,0.733381167783709,
1.68520781074188));
#30047=CARTESIAN_POINT('Ctrl Pts',(-4.09976430380214,-1.01649372201922,
1.53118053009453));
#30048=CARTESIAN_POINT('Ctrl Pts',(-3.98874280672331,-1.83774423197443,
-0.0216665754003948));
#30049=CARTESIAN_POINT('Ctrl Pts',(-3.87772130964449,-0.980111674806025,
-1.55472004153636));
#30050=CARTESIAN_POINT('Ctrl Pts',(-3.76669981256566,0.772908208897534,
-1.66744901069363));
#30051=CARTESIAN_POINT('Ctrl Pts',(-3.65567831548684,1.81983282548855,-0.256869207804794));
#30052=CARTESIAN_POINT('Ctrl Pts',(-3.54465681840801,1.20423745559398,1.38837511256683));
#30053=CARTESIAN_POINT('Ctrl Pts',(-3.43363532132918,-0.511496789897079,
1.76526041607566));
#30054=CARTESIAN_POINT('Ctrl Pts',(-3.32261382425036,-1.75994985201377,
0.529480708842188));
#30055=CARTESIAN_POINT('Ctrl Pts',(-3.21159232717153,-1.40058940335731,
-1.19000950663588));
#30056=CARTESIAN_POINT('Ctrl Pts',(-3.1005708300927,0.238288506115619,-1.82235888080426));
#30057=CARTESIAN_POINT('Ctrl Pts',(-2.98954933301389,1.65947641764626,-0.789880574454531));
#30058=CARTESIAN_POINT('Ctrl Pts',(-2.87852783593505,1.5646389708752,0.964198212866461));
#30059=CARTESIAN_POINT('Ctrl Pts',(-2.76750633885623,0.0404155252740006,
1.83742751899441));
#30060=CARTESIAN_POINT('Ctrl Pts',(-2.6564848417774,-1.52072978321424,1.03206309355985));
#30061=CARTESIAN_POINT('Ctrl Pts',(-2.54546334469858,-1.69260261440109,
-0.716149211990789));
#30062=CARTESIAN_POINT('Ctrl Pts',(-2.43444184761975,-0.31818743609586,
-1.81011879586092));
#30063=CARTESIAN_POINT('Ctrl Pts',(-2.32342035054093,1.34690991987603,-1.25044271013452));
#30064=CARTESIAN_POINT('Ctrl Pts',(-2.2123988534621,1.78152905596337,0.45158336374919));
#30065=CARTESIAN_POINT('Ctrl Pts',(-2.10137735638328,0.588620854178164,
1.74106254069739));
#30066=CARTESIAN_POINT('Ctrl Pts',(-1.99035585930445,-1.14202570378047,
1.43998284972631));
#30067=CARTESIAN_POINT('Ctrl Pts',(-1.87933436222563,-1.82936735575706,
-0.176602472857783));
#30068=CARTESIAN_POINT('Ctrl Pts',(-1.7683128651468,-0.845478645101226,
-1.63185140458178));
#30069=CARTESIAN_POINT('Ctrl Pts',(-1.65729136806797,0.910802436555798,
-1.59631211106002));
#30070=CARTESIAN_POINT('Ctrl Pts',(-1.54626987098914,1.83501425402401,-0.102451380513119));
#30071=CARTESIAN_POINT('Ctrl Pts',(-1.43524837391032,1.08283668534245,1.48500401619214));
#30072=CARTESIAN_POINT('Ctrl Pts',(-1.32422687683149,-0.658572718107321,
1.71582529904111));
#30073=CARTESIAN_POINT('Ctrl Pts',(-1.21320537975267,-1.79833989307757,
0.379141704382714));
#30074=CARTESIAN_POINT('Ctrl Pts',(-1.10218388267384,-1.29521996548735,
-1.30390612015762));
#30075=CARTESIAN_POINT('Ctrl Pts',(-0.991162385595018,0.391152455034581,
-1.79576804489885));
#30076=CARTESIAN_POINT('Ctrl Pts',(-0.880140888516193,1.72019272226962,
-0.647083240986163));
#30077=CARTESIAN_POINT('Ctrl Pts',(-0.769119391437366,1.47772522761866,
1.09272715853592));
#30078=CARTESIAN_POINT('Ctrl Pts',(-0.658097894358541,-0.114699807832016,
1.83431047841002));
#30079=CARTESIAN_POINT('Ctrl Pts',(-0.547076397279716,-1.60239309641882,
0.900069920860329));
#30080=CARTESIAN_POINT('Ctrl Pts',(-0.43605490020089,-1.62610899044603,
-0.856287353085414));
#30081=CARTESIAN_POINT('Ctrl Pts',(-0.325033403122065,-0.164474555116665,
-1.83065940731556));
#30082=CARTESIAN_POINT('Ctrl Pts',(-0.21401190604324,1.4477823064221,-1.13208461653888));
#30083=CARTESIAN_POINT('Ctrl Pts',(-0.102990408964413,1.73671048154547,
0.599690938180032));
#30084=CARTESIAN_POINT('Ctrl Pts',(0.00803108811441221,0.440400782633002,
1.78557817668643));
#30085=CARTESIAN_POINT('Ctrl Pts',(0.119052585193236,-1.26094589866601,
1.33635313142488));
#30086=CARTESIAN_POINT('Ctrl Pts',(0.193066916579123,-1.62303132195317,
0.228752033396824));
#30087=CARTESIAN_POINT('Ctrl Pts',(0.230074082272065,-1.53017656606561,
-0.279535197539876));
#30088=CARTESIAN_POINT('',(0.,-1.92218901323832,-0.351148682734097));
#30089=CARTESIAN_POINT('Ctrl Pts',(1.0547118733939E-15,0.480182858679996,
1.4822056829043));
#30090=CARTESIAN_POINT('Ctrl Pts',(1.40003008271787E-15,0.446073771342386,
1.49837437681773));
#30091=CARTESIAN_POINT('Ctrl Pts',(3.73246695668943E-15,0.411402367961804,
1.5131874054692));
#30092=CARTESIAN_POINT('Ctrl Pts',(2.692290834716E-15,0.376229275515442,
1.52659018558423));
#30093=CARTESIAN_POINT('Ctrl Pts',(1.05407315971151E-15,0.320788673731233,
1.54771594233397));
#30094=CARTESIAN_POINT('Ctrl Pts',(-4.67470066845617E-15,0.264103101937485,
1.56534066809337));
#30095=CARTESIAN_POINT('Ctrl Pts',(-7.49400541621981E-15,0.206476417853331,
1.57959203319563));
#30096=CARTESIAN_POINT('Ctrl Pts',(-9.15600442216292E-15,0.172505102145218,
1.58799330824477));
#30097=CARTESIAN_POINT('Ctrl Pts',(-4.65850075858084E-15,0.138206098176861,
1.59522147264912));
#30098=CARTESIAN_POINT('Ctrl Pts',(-4.46864767411626E-15,0.1036374144592,
1.60129566587682));
#30099=CARTESIAN_POINT('Ctrl Pts',(-4.38277324586137E-15,0.0880012926750868,
1.60404314755197));
#30100=CARTESIAN_POINT('Ctrl Pts',(-1.04319479122915E-14,0.0723076512843924,
1.60655463309822));
#30101=CARTESIAN_POINT('Ctrl Pts',(-9.96425164601078E-15,0.0565846426208889,
1.60882871578729));
#30102=CARTESIAN_POINT('Ctrl Pts',(-8.12965378682446E-15,-0.00509085088565643,
1.61774909324972));
#30103=CARTESIAN_POINT('Ctrl Pts',(-4.56836786455393E-15,-0.0672895814378321,
1.62303444302115));
#30104=CARTESIAN_POINT('Ctrl Pts',(-3.94129173741931E-15,-0.129678743792337,
1.62482203126307));
#30105=CARTESIAN_POINT('Ctrl Pts',(-3.45837203070848E-15,-0.177725471585729,
1.62619867686024));
#30106=CARTESIAN_POINT('Ctrl Pts',(-8.22270713878231E-15,-0.225885969277299,
1.62549994364171));
#30107=CARTESIAN_POINT('Ctrl Pts',(-9.35362898246694E-15,-0.274016954341825,
1.62276943393303));
#30108=CARTESIAN_POINT('Ctrl Pts',(-9.74287591606784E-15,-0.290582942922006,
1.62182963200312));
#30109=CARTESIAN_POINT('Ctrl Pts',(-5.84326107154292E-15,-0.307145480266589,
1.62064899356115));
#30110=CARTESIAN_POINT('Ctrl Pts',(-5.77315972805081E-15,-0.32369883547967,
1.61922884021275));
#30111=CARTESIAN_POINT('Ctrl Pts',(-5.70623215198899E-15,-0.339502754276557,
1.61787298287094));
#30112=CARTESIAN_POINT('Ctrl Pts',(-7.88705881085276E-15,-0.355302127669727,
1.61629822797713));
#30113=CARTESIAN_POINT('Ctrl Pts',(-7.85482789922298E-15,-0.37106496199202,
1.6145090262086));
#30114=CARTESIAN_POINT('Ctrl Pts',(-7.72335550546971E-15,-0.435362788392118,
1.60721073312527));
#30115=CARTESIAN_POINT('Ctrl Pts',(-3.55546619181194E-15,-0.499135001074743,
1.59634267751575));
#30116=CARTESIAN_POINT('Ctrl Pts',(-3.41393580072236E-15,-0.562042543794224,
1.58204256350879));
#30117=CARTESIAN_POINT('Ctrl Pts',(-3.26945119203353E-15,-0.626263179541966,
1.56744395779171));
#30118=CARTESIAN_POINT('Ctrl Pts',(-5.59097293134417E-15,-0.689583748551309,
1.54926866320265));
#30119=CARTESIAN_POINT('Ctrl Pts',(-6.02295990859147E-15,-0.751656795048653,
1.52761115641076));
#30120=CARTESIAN_POINT('Ctrl Pts',(-6.30853923919458E-15,-0.792692242876652,
1.5132937426508));
#30121=CARTESIAN_POINT('Ctrl Pts',(-8.12105679605289E-15,-0.833182736037355,
1.49745341724689));
#30122=CARTESIAN_POINT('Ctrl Pts',(-8.77076189453874E-15,-0.873027345587097,
1.48010498047163));
#30123=CARTESIAN_POINT('Ctrl Pts',(-9.08990039389072E-15,-0.892599223549276,
1.471583338743));
#30124=CARTESIAN_POINT('Ctrl Pts',(-4.31109323122687E-15,-0.912015235103237,
1.46269766499479));
#30125=CARTESIAN_POINT('Ctrl Pts',(-4.44089209850063E-15,-0.931263178081411,
1.45344884058705));
#30126=CARTESIAN_POINT('Ctrl Pts',(-4.52342416443145E-15,-0.943501901979956,
1.44756801433768));
#30127=CARTESIAN_POINT('Ctrl Pts',(-6.71139558524068E-15,-0.955672671980721,
1.4415403547937));
#30128=CARTESIAN_POINT('Ctrl Pts',(-6.9111383282916E-15,-0.967772301054401,
1.43536596810798));
#30129=CARTESIAN_POINT('Ctrl Pts',(-7.06505675977478E-15,-0.977096073723701,
1.4306080885499));
#30130=CARTESIAN_POINT('Ctrl Pts',(-7.66117988453509E-15,-0.986374557138314,
1.42576457472066));
#30131=CARTESIAN_POINT('Ctrl Pts',(-7.38298311375729E-15,-0.995598865169279,
1.42083978831382));
#30132=CARTESIAN_POINT('Ctrl Pts',(-5.5803017413817E-15,-1.05537126372727,
1.38892776901282));
#30133=CARTESIAN_POINT('Ctrl Pts',(3.49033535941956E-16,-1.11296260466219,
1.35355987724473));
#30134=CARTESIAN_POINT('Ctrl Pts',(-5.55111512312578E-17,-1.16801443157665,
1.31484833578652));
#30135=CARTESIAN_POINT('Ctrl Pts',(-1.58292162970789E-16,-1.18200122376002,
1.30501305300262));
#30136=CARTESIAN_POINT('Ctrl Pts',(-8.42000433806714E-15,-1.19582408399153,
1.29496167698215));
#30137=CARTESIAN_POINT('Ctrl Pts',(-8.2572837456496E-15,-1.20947707828799,
1.28469551483091));
#30138=CARTESIAN_POINT('Ctrl Pts',(-7.63946596890415E-15,-1.2613147864529,
1.24571693577246));
#30139=CARTESIAN_POINT('Ctrl Pts',(-3.87298011944514E-15,-1.31070559621982,
1.20364581809758));
#30140=CARTESIAN_POINT('Ctrl Pts',(-3.05311331771918E-15,-1.35758932481216,
1.15879636045725));
#30141=CARTESIAN_POINT('Ctrl Pts',(-2.60837798406203E-15,-1.38302132258876,
1.13446784945275));
#30142=CARTESIAN_POINT('Ctrl Pts',(-3.43302993469709E-15,-1.40771522401955,
1.10932096817457));
#30143=CARTESIAN_POINT('Ctrl Pts',(-3.6498581934552E-15,-1.43165822803284,
1.08340051001308));
#30144=CARTESIAN_POINT('Ctrl Pts',(-3.8156193117322E-15,-1.44996220345968,
1.06358480814972));
#30145=CARTESIAN_POINT('Ctrl Pts',(-2.87284372802704E-15,-1.46782728641225,
1.04331692584045));
#30146=CARTESIAN_POINT('Ctrl Pts',(-3.1641356201817E-15,-1.48524671954972,
1.02261561267638));
#30147=CARTESIAN_POINT('Ctrl Pts',(-3.32383551962965E-15,-1.49479687111733,
1.01126618030362));
#30148=CARTESIAN_POINT('Ctrl Pts',(-6.89733966939696E-15,-1.50421538093661,
0.999783335138857));
#30149=CARTESIAN_POINT('Ctrl Pts',(-6.74460487459783E-15,-1.51348427825112,
0.988191590561737));
#30150=CARTESIAN_POINT('Ctrl Pts',(-6.04666371398387E-15,-1.55583968886863,
0.935221632574525));
#30151=CARTESIAN_POINT('Ctrl Pts',(-3.0413638622061E-15,-1.59514251466625,
0.879902068251074));
#30152=CARTESIAN_POINT('Ctrl Pts',(-2.94209101525666E-15,-1.6313405550829,
0.822591921935408));
#30153=CARTESIAN_POINT('Ctrl Pts',(-2.84072911148816E-15,-1.66830033212234,
0.764075764553859));
#30154=CARTESIAN_POINT('Ctrl Pts',(-2.77218863047414E-15,-1.70202388244217,
0.703483705813104));
#30155=CARTESIAN_POINT('Ctrl Pts',(-2.85188539450587E-15,-1.73242530624915,
0.641151720491997));
#30156=CARTESIAN_POINT('Ctrl Pts',(-2.93218559451239E-15,-1.76305691898579,
0.578347779216597));
#30157=CARTESIAN_POINT('Ctrl Pts',(-2.99436507783698E-15,-1.79031650407563,
0.513776618683869));
#30158=CARTESIAN_POINT('Ctrl Pts',(-3.77475828372553E-15,-1.81407668145728,
0.447747080004075));
#30159=CARTESIAN_POINT('Ctrl Pts',(-3.97176467194236E-15,-1.8200748202084,
0.431078250966644));
#30160=CARTESIAN_POINT('Ctrl Pts',(-5.93455269918665E-15,-1.82584972626931,
0.414316345880479));
#30161=CARTESIAN_POINT('Ctrl Pts',(-6.07153216591882E-15,-1.83139888490863,
0.397466087487765));
#30162=CARTESIAN_POINT('Ctrl Pts',(-6.17145811240212E-15,-1.8354469728626,
0.385173894660996));
#30163=CARTESIAN_POINT('Ctrl Pts',(-3.09749045409741E-15,-1.83937529592778,
0.37283314186271));
#30164=CARTESIAN_POINT('Ctrl Pts',(-2.82412981889024E-15,-1.84317748112416,
0.360463942797997));
#30165=CARTESIAN_POINT('Ctrl Pts',(-1.2991746729061E-15,-1.86438814986878,
0.291461784710604));
#30166=CARTESIAN_POINT('Ctrl Pts',(1.37739593958821E-15,-1.88171855913059,
0.221453627220656));
#30167=CARTESIAN_POINT('Ctrl Pts',(1.30451205393456E-15,-1.89508700640948,
0.150800366152206));
#30168=CARTESIAN_POINT('Ctrl Pts',(1.23145509346081E-15,-1.90848719927364,
0.0799793272500314));
#30169=CARTESIAN_POINT('Ctrl Pts',(-1.27203037467893E-15,-1.91790714514985,
0.00850916986176715));
#30170=CARTESIAN_POINT('Ctrl Pts',(-2.42167397246362E-15,-1.92322202108538,
-0.0632768841144876));
#30171=CARTESIAN_POINT('Ctrl Pts',(-3.54683445949221E-15,-1.92842371003285,
-0.133534163509098));
#30172=CARTESIAN_POINT('Ctrl Pts',(-4.48891627368549E-15,-1.92969366211441,
-0.204094995398863));
#30173=CARTESIAN_POINT('Ctrl Pts',(-6.6040922730437E-15,-1.9268677763229,
-0.274661643730342));
#30174=CARTESIAN_POINT('Ctrl Pts',(-7.36841819229932E-15,-1.92584663304406,
-0.300161138037724));
#30175=CARTESIAN_POINT('Ctrl Pts',(3.63423914059134E-17,-1.92429019227826,
-0.325661462754304));
#30176=CARTESIAN_POINT('Ctrl Pts',(0.,-1.92218901323832,-0.351148682734097));
#30177=CARTESIAN_POINT('Ctrl Pts',(0.,-1.92218901323832,-0.351148682734097));
#30178=CARTESIAN_POINT('Ctrl Pts',(-0.00671010262525542,-1.94333860721344,
-0.235375737618954));
#30179=CARTESIAN_POINT('Ctrl Pts',(-0.0134202052505109,-1.9531764658261,
-0.117723130693868));
#30180=CARTESIAN_POINT('Ctrl Pts',(-0.0201303078757663,-1.95230810266922,
-4.45419903166711E-5));
#30181=CARTESIAN_POINT('Origin',(-7.7,0.,0.));
#30182=CARTESIAN_POINT('Origin',(0.,0.,0.));
#30183=CARTESIAN_POINT('Origin',(-16.,1.6,0.));
#30184=CARTESIAN_POINT('',(-16.,-1.6,-1.95943487863577E-16));
#30185=CARTESIAN_POINT('Origin',(-16.,0.,0.));
#30186=CARTESIAN_POINT('Origin',(-15.8,0.,0.));
#30187=CARTESIAN_POINT('',(-15.8,-1.8,-2.20436423846524E-16));
#30188=CARTESIAN_POINT('Origin',(2.51157561548264,0.,0.));
#30189=CARTESIAN_POINT('',(2.38930775492008,3.5,-2.02072594216369));
#30190=CARTESIAN_POINT('',(2.38930775492008,-7.42402667107435E-16,-4.04145188432738));
#30191=CARTESIAN_POINT('Ctrl Pts',(2.38930775492008,3.5,-2.02072594216369));
#30192=CARTESIAN_POINT('Ctrl Pts',(2.98258118464813,1.75,-3.03108891324554));
#30193=CARTESIAN_POINT('Ctrl Pts',(2.38930775492008,-7.42402667107435E-16,
-4.04145188432738));
#30194=CARTESIAN_POINT('',(2.38930775492008,3.5,2.02072594216369));
#30195=CARTESIAN_POINT('Ctrl Pts',(2.38930775492008,3.5,2.02072594216369));
#30196=CARTESIAN_POINT('Ctrl Pts',(2.98258118464813,3.5,-3.60822483003176E-15));
#30197=CARTESIAN_POINT('Ctrl Pts',(2.38930775492008,3.5,-2.02072594216369));
#30198=CARTESIAN_POINT('',(2.38930775492008,2.47467555702478E-16,4.04145188432738));
#30199=CARTESIAN_POINT('Ctrl Pts',(2.38930775492008,2.47467555702478E-16,
4.04145188432738));
#30200=CARTESIAN_POINT('Ctrl Pts',(2.98258118464813,1.75,3.03108891324553));
#30201=CARTESIAN_POINT('Ctrl Pts',(2.38930775492008,3.5,2.02072594216369));
#30202=CARTESIAN_POINT('',(2.38930775492008,-3.5,2.02072594216369));
#30203=CARTESIAN_POINT('Ctrl Pts',(2.38930775492008,-3.5,2.02072594216369));
#30204=CARTESIAN_POINT('Ctrl Pts',(2.98258118464813,-1.75,3.03108891324554));
#30205=CARTESIAN_POINT('Ctrl Pts',(2.38930775492008,2.47467555702478E-16,
4.04145188432738));
#30206=CARTESIAN_POINT('',(2.70724202769303,-3.5,-4.31113475248839E-16));
#30207=CARTESIAN_POINT('Ctrl Pts',(2.70724202769303,-3.5,-4.33600570796104E-16));
#30208=CARTESIAN_POINT('Ctrl Pts',(2.70724202769303,-3.5,0.937822173508931));
#30209=CARTESIAN_POINT('Ctrl Pts',(2.38930775492008,-3.5,2.02072594216369));
#30210=CARTESIAN_POINT('',(2.8,-3.34203030879952,-4.09280672032477E-16));
#30211=CARTESIAN_POINT('',(2.51157561548264,-3.83322594216369,-4.69434788047936E-16));
#30212=CARTESIAN_POINT('Origin',(2.8,0.,0.));
#30213=CARTESIAN_POINT('',(2.38930775492008,-3.5,-2.02072594216369));
#30214=CARTESIAN_POINT('Ctrl Pts',(2.38930775492008,-3.5,-2.02072594216369));
#30215=CARTESIAN_POINT('Ctrl Pts',(2.70724202769302,-3.5,-0.93782217350893));
#30216=CARTESIAN_POINT('Ctrl Pts',(2.70724202769303,-3.5,-4.33600570796104E-16));
#30217=CARTESIAN_POINT('Ctrl Pts',(2.38930775492008,-7.42402667107435E-16,
-4.04145188432738));
#30218=CARTESIAN_POINT('Ctrl Pts',(2.98258118464813,-1.75,-3.03108891324553));
#30219=CARTESIAN_POINT('Ctrl Pts',(2.38930775492008,-3.5,-2.02072594216369));
#30220=CARTESIAN_POINT('Origin',(0.,2.47467555702478E-16,4.04145188432738));
#30221=CARTESIAN_POINT('',(0.,2.47467555702478E-16,4.04145188432738));
#30222=CARTESIAN_POINT('',(0.,2.47467555702478E-16,4.04145188432738));
#30223=CARTESIAN_POINT('',(0.,-3.5,2.02072594216369));
#30224=CARTESIAN_POINT('',(0.,2.47467555702478E-16,4.04145188432738));
#30225=CARTESIAN_POINT('',(0.,-3.5,2.02072594216369));
#30226=CARTESIAN_POINT('Origin',(0.,3.5,2.02072594216369));
#30227=CARTESIAN_POINT('',(0.,3.5,2.02072594216369));
#30228=CARTESIAN_POINT('',(0.,3.5,2.02072594216369));
#30229=CARTESIAN_POINT('',(0.,3.5,2.02072594216369));
#30230=CARTESIAN_POINT('Origin',(0.,3.5,-2.02072594216369));
#30231=CARTESIAN_POINT('',(0.,3.5,-2.02072594216369));
#30232=CARTESIAN_POINT('',(0.,3.5,-2.02072594216369));
#30233=CARTESIAN_POINT('',(0.,3.5,-2.02072594216369));
#30234=CARTESIAN_POINT('Origin',(0.,-7.42402667107435E-16,-4.04145188432738));
#30235=CARTESIAN_POINT('',(0.,-7.42402667107435E-16,-4.04145188432738));
#30236=CARTESIAN_POINT('',(0.,-7.42402667107435E-16,-4.04145188432738));
#30237=CARTESIAN_POINT('',(0.,-7.42402667107435E-16,-4.04145188432738));
#30238=CARTESIAN_POINT('Origin',(0.,-3.5,-2.02072594216369));
#30239=CARTESIAN_POINT('',(0.,-3.5,-2.02072594216369));
#30240=CARTESIAN_POINT('',(0.,-3.5,-2.02072594216369));
#30241=CARTESIAN_POINT('',(0.,-3.5,-2.02072594216369));
#30242=CARTESIAN_POINT('Origin',(0.,-3.5,2.02072594216369));
#30243=CARTESIAN_POINT('',(0.,-3.5,2.02072594216369));
#30244=CARTESIAN_POINT('Origin',(2.8,0.,0.));
#30245=CARTESIAN_POINT('Origin',(0.,0.,0.));
#30246=CARTESIAN_POINT('',(0.,0.,0.));
#30247=CARTESIAN_POINT('Origin',(-9.8,0.,0.));
#30248=CARTESIAN_POINT('',(-19.4201303078758,-1.95628952807724,0.00129327600707104));
#30249=CARTESIAN_POINT('',(-19.5218696921242,-1.95584467742209,0.00207536885323489));
#30250=CARTESIAN_POINT('',(-9.8,-1.954,-2.39295984553393E-16));
#30251=CARTESIAN_POINT('',(-19.646,0.862546313953447,1.75510541481596));
#30252=CARTESIAN_POINT('Ctrl Pts',(-19.4201303078758,-1.95628952807724,
0.00129327600707104));
#30253=CARTESIAN_POINT('Ctrl Pts',(-19.4240588726576,-1.95677268946339,
0.069961262552598));
#30254=CARTESIAN_POINT('Ctrl Pts',(-19.4279874374395,-1.95347076783648,
0.138579280748551));
#30255=CARTESIAN_POINT('Ctrl Pts',(-19.4319160022213,-1.94623009822624,
0.206775368035542));
#30256=CARTESIAN_POINT('Ctrl Pts',(-19.4689291755589,-1.87801176042438,
0.849288280477544));
#30257=CARTESIAN_POINT('Ctrl Pts',(-19.5059423488964,-1.4601680051776,1.45434823304434));
#30258=CARTESIAN_POINT('Ctrl Pts',(-19.542955522234,-0.883489447908455,
1.7462425910547));
#30259=CARTESIAN_POINT('Ctrl Pts',(-19.5773036814893,-0.348332768864228,
2.01712003793654));
#30260=CARTESIAN_POINT('Ctrl Pts',(-19.6116518407447,0.323609377828236,
2.01830531561287));
#30261=CARTESIAN_POINT('Ctrl Pts',(-19.646,0.8635667682364,1.75638951800437));
#30262=CARTESIAN_POINT('',(-19.646,-0.861525859670563,1.75382131162753));
#30263=CARTESIAN_POINT('Origin',(-19.646,0.,0.));
#30264=CARTESIAN_POINT('Ctrl Pts',(-19.646,-0.861525859670562,1.75382131162753));
#30265=CARTESIAN_POINT('Ctrl Pts',(-19.6089868266624,-1.44419697921243,
1.46759703447886));
#30266=CARTESIAN_POINT('Ctrl Pts',(-19.5719736533249,-1.86803384659668,
0.870718499491397));
#30267=CARTESIAN_POINT('Ctrl Pts',(-19.5349604799873,-1.94348346552551,
0.229996089379168));
#30268=CARTESIAN_POINT('Ctrl Pts',(-19.5305968840329,-1.95237845134348,
0.154459369219161));
#30269=CARTESIAN_POINT('Ctrl Pts',(-19.5262332880786,-1.95643128236097,
0.0783132730520005));
#30270=CARTESIAN_POINT('Ctrl Pts',(-19.5218696921242,-1.95584467742209,
0.00207536885323489));
#30271=CARTESIAN_POINT('Origin',(-9.8,0.,0.));
#30272=CARTESIAN_POINT('',(-18.7201303078758,-1.95122552025463,0.000915013127814612));
#30273=CARTESIAN_POINT('',(-18.8218696921242,-1.95111957186981,0.000817319826409989));
#30274=CARTESIAN_POINT('',(-9.8,-1.954,-2.39295984553393E-16));
#30275=CARTESIAN_POINT('Ctrl Pts',(-18.7201303078758,-1.95122552025463,
0.000915013127814612));
#30276=CARTESIAN_POINT('Ctrl Pts',(-18.7353131659656,-1.95235483286073,
0.268087242358252));
#30277=CARTESIAN_POINT('Ctrl Pts',(-18.7504960240554,-1.90126484018336,
0.534845561933385));
#30278=CARTESIAN_POINT('Ctrl Pts',(-18.7656788821451,-1.79588180634386,
0.778079849513106));
#30279=CARTESIAN_POINT('Ctrl Pts',(-18.8026920554827,-1.53897625698858,
1.37104283412289));
#30280=CARTESIAN_POINT('Ctrl Pts',(-18.8397052288203,-0.959407278208984,
1.8242025460654));
#30281=CARTESIAN_POINT('Ctrl Pts',(-18.8767184021578,-0.321985378344434,
1.93051955012324));
#30282=CARTESIAN_POINT('Ctrl Pts',(-18.9137315754954,0.315436521520117,
2.03683655418109));
#30283=CARTESIAN_POINT('Ctrl Pts',(-18.950744748833,1.01071134246962,1.79631085035426));
#30284=CARTESIAN_POINT('Ctrl Pts',(-18.9877579221705,1.44615311561289,1.31881232311228));
#30285=CARTESIAN_POINT('Ctrl Pts',(-19.0247710955081,1.88159488875616,0.84131379587029));
#30286=CARTESIAN_POINT('Ctrl Pts',(-19.0617842688456,2.05720361409319,0.126842445213142));
#30287=CARTESIAN_POINT('Ctrl Pts',(-19.0987974421832,1.89275097145487,-0.498093241961312));
#30288=CARTESIAN_POINT('Ctrl Pts',(-19.1358106155208,1.72829832881656,-1.12302892913577));
#30289=CARTESIAN_POINT('Ctrl Pts',(-19.1728237888583,1.22378431820289,-1.65842895282753));
#30290=CARTESIAN_POINT('Ctrl Pts',(-19.2098369621959,0.609709882174192,
-1.85976901676034));
#30291=CARTESIAN_POINT('Ctrl Pts',(-19.2468501355335,-0.00436455385450528,
-2.06110908069315));
#30292=CARTESIAN_POINT('Ctrl Pts',(-19.283863308871,-0.727999415298231,
-1.92838918486701));
#30293=CARTESIAN_POINT('Ctrl Pts',(-19.3208764822086,-1.23052038584163,
-1.52204630079534));
#30294=CARTESIAN_POINT('Ctrl Pts',(-19.3539610907643,-1.67970396299246,
-1.15883250293187));
#30295=CARTESIAN_POINT('Ctrl Pts',(-19.3870456993201,-1.95222055983625,
-0.576997672807184));
#30296=CARTESIAN_POINT('Ctrl Pts',(-19.4201303078758,-1.95628952807724,
0.00129327600707104));
#30297=CARTESIAN_POINT('Ctrl Pts',(-19.5218696921242,-1.95584467742209,
0.00207536885323489));
#30298=CARTESIAN_POINT('Ctrl Pts',(-19.489220114741,-1.95145554434339,-0.568356765264027));
#30299=CARTESIAN_POINT('Ctrl Pts',(-19.4565705373578,-1.68733094748134,
-1.14392870557586));
#30300=CARTESIAN_POINT('Ctrl Pts',(-19.4239209599746,-1.24838760910815,
-1.50783684792128));
#30301=CARTESIAN_POINT('Ctrl Pts',(-19.386907786637,-0.750779763288562,
-1.92038108987251));
#30302=CARTESIAN_POINT('Ctrl Pts',(-19.3498946132995,-0.0285017011759892,
-2.06090328853796));
#30303=CARTESIAN_POINT('Ctrl Pts',(-19.3128814399619,0.587948268210155,
-1.86661002179603));
#30304=CARTESIAN_POINT('Ctrl Pts',(-19.2758682666244,1.2043982375963,-1.6723167550541));
#30305=CARTESIAN_POINT('Ctrl Pts',(-19.2388550932868,1.71502011425601,-1.14320802290478));
#30306=CARTESIAN_POINT('Ctrl Pts',(-19.2018419199492,1.8867513877996,-0.520323693783771));
#30307=CARTESIAN_POINT('Ctrl Pts',(-19.1648287466117,2.0584826613432,0.102560635337238));
#30308=CARTESIAN_POINT('Ctrl Pts',(-19.1278155732741,1.89132333177067,0.819220561429935));
#30309=CARTESIAN_POINT('Ctrl Pts',(-19.0908023999365,1.46152107494396,1.30183002295279));
#30310=CARTESIAN_POINT('Ctrl Pts',(-19.053789226599,1.03171881811726,1.78443948447564));
#30311=CARTESIAN_POINT('Ctrl Pts',(-19.0167760532614,0.339273634036384,
2.03299848142864));
#30312=CARTESIAN_POINT('Ctrl Pts',(-18.9797628799238,-0.299358392794465,
1.93413318743984));
#30313=CARTESIAN_POINT('Ctrl Pts',(-18.9427497065863,-0.937990419625319,
1.83526789345104));
#30314=CARTESIAN_POINT('Ctrl Pts',(-18.9057365332487,-1.52280928920615,
1.38897830852044));
#30315=CARTESIAN_POINT('Ctrl Pts',(-18.8687233599112,-1.78663886004406,
0.799077292011544));
#30316=CARTESIAN_POINT('Ctrl Pts',(-18.8531054706488,-1.89796303600405,
0.550165677016122));
#30317=CARTESIAN_POINT('Ctrl Pts',(-18.8374875813865,-1.95213637563171,
0.275684631968902));
#30318=CARTESIAN_POINT('Ctrl Pts',(-18.8218696921242,-1.95111957186981,
0.000817319826409989));
#30319=CARTESIAN_POINT('Origin',(-9.8,0.,0.));
#30320=CARTESIAN_POINT('',(-18.0201303078758,-1.95299307732975,-0.00171153559867271));
#30321=CARTESIAN_POINT('',(-18.1218696921242,-1.95320927907148,-0.00174204714352619));
#30322=CARTESIAN_POINT('',(-9.8,-1.954,-2.39295984553393E-16));
#30323=CARTESIAN_POINT('Ctrl Pts',(-18.0201303078758,-1.95299307732975,
-0.00171153559867271));
#30324=CARTESIAN_POINT('Ctrl Pts',(-18.0465674592735,-1.94907576194016,
0.462441490461123));
#30325=CARTESIAN_POINT('Ctrl Pts',(-18.0730046106712,-1.78336958701272,
0.929108469286399));
#30326=CARTESIAN_POINT('Ctrl Pts',(-18.099441762069,-1.48183519126904,1.27857813100852));
#30327=CARTESIAN_POINT('Ctrl Pts',(-18.1364549354065,-1.05967379085981,
1.76785100957778));
#30328=CARTESIAN_POINT('Ctrl Pts',(-18.1734681087441,-0.371272370021996,
2.02740273070118));
#30329=CARTESIAN_POINT('Ctrl Pts',(-18.2104812820817,0.268828848722206,
1.93864079577349));
#30330=CARTESIAN_POINT('Ctrl Pts',(-18.2474944554192,0.908930067466409,
1.84987886084581));
#30331=CARTESIAN_POINT('Ctrl Pts',(-18.2845076287568,1.50073108411699,1.41280326986704));
#30332=CARTESIAN_POINT('Ctrl Pts',(-18.3215208020944,1.77382959268256,0.827119374505746));
#30333=CARTESIAN_POINT('Ctrl Pts',(-18.3585339754319,2.04692810124813,0.24143547914445));
#30334=CARTESIAN_POINT('Ctrl Pts',(-18.3955471487695,2.00132410172869,-0.492856720599384));
#30335=CARTESIAN_POINT('Ctrl Pts',(-18.4325603221071,1.65785490807018,-1.04024761341585));
#30336=CARTESIAN_POINT('Ctrl Pts',(-18.4695734954446,1.31438571441166,-1.58763850623231));
#30337=CARTESIAN_POINT('Ctrl Pts',(-18.5065866687822,0.673051326614071,
-1.94812809212141));
#30338=CARTESIAN_POINT('Ctrl Pts',(-18.5435998421197,0.0268860436523521,
-1.95700588033934));
#30339=CARTESIAN_POINT('Ctrl Pts',(-18.5806130154573,-0.619279239309369,
-1.96588366855727));
#30340=CARTESIAN_POINT('Ctrl Pts',(-18.6176261887949,-1.27027541743522,
-1.62314965910403));
#30341=CARTESIAN_POINT('Ctrl Pts',(-18.6546393621324,-1.62865244653266,
-1.08539952573888));
#30342=CARTESIAN_POINT('Ctrl Pts',(-18.6764696773802,-1.84002269169937,
-0.768235287243793));
#30343=CARTESIAN_POINT('Ctrl Pts',(-18.698299992628,-1.94960176469699,-0.3832322900387));
#30344=CARTESIAN_POINT('Ctrl Pts',(-18.7201303078758,-1.95122552025463,
0.000915013127814612));
#30345=CARTESIAN_POINT('Ctrl Pts',(-18.8218696921242,-1.95111957186981,
0.000817319826409989));
#30346=CARTESIAN_POINT('Ctrl Pts',(-18.800474408049,-1.94972663041856,-0.375729352231495));
#30347=CARTESIAN_POINT('Ctrl Pts',(-18.7790791239737,-1.84475916201458,
-0.753000926042014));
#30348=CARTESIAN_POINT('Ctrl Pts',(-18.7576838398985,-1.64125793500757,
-1.06625371430635));
#30349=CARTESIAN_POINT('Ctrl Pts',(-18.7206706665609,-1.28920716703816,
-1.60817125602816));
#30350=CARTESIAN_POINT('Ctrl Pts',(-18.6836574932233,-0.642265359004347,
-1.95849389138462));
#30351=CARTESIAN_POINT('Ctrl Pts',(-18.6466443198858,0.00396079527596547,
-1.95718277265247));
#30352=CARTESIAN_POINT('Ctrl Pts',(-18.6096311465482,0.650186949556277,
-1.95587165392032));
#30353=CARTESIAN_POINT('Ctrl Pts',(-18.5726179732106,1.29569745008309,-1.60292678109958));
#30354=CARTESIAN_POINT('Ctrl Pts',(-18.5356047998731,1.64555468172952,-1.05959865244045));
#30355=CARTESIAN_POINT('Ctrl Pts',(-18.4985916265355,1.99541191337596,-0.516270523781318));
#30356=CARTESIAN_POINT('Ctrl Pts',(-18.4615784531979,2.04961587614203,0.2174408607162));
#30357=CARTESIAN_POINT('Ctrl Pts',(-18.4245652798604,1.78339728471467,0.80628459334565));
#30358=CARTESIAN_POINT('Ctrl Pts',(-18.3875521065228,1.51717869328732,1.3951283259751));
#30359=CARTESIAN_POINT('Ctrl Pts',(-18.3505389331852,0.930537547666546,
1.83910440673648));
#30360=CARTESIAN_POINT('Ctrl Pts',(-18.3135257598477,0.291519864690383,
1.93535806385024));
#30361=CARTESIAN_POINT('Ctrl Pts',(-18.2765125865101,-0.34749781828578,
2.03161172096399));
#30362=CARTESIAN_POINT('Ctrl Pts',(-18.2394994131726,-1.03889203861734,
1.78014295443012));
#30363=CARTESIAN_POINT('Ctrl Pts',(-18.202486239835,-1.46675581987468,1.29584920213102));
#30364=CARTESIAN_POINT('Ctrl Pts',(-18.1756140572647,-1.77739207741162,
0.944243842311544));
#30365=CARTESIAN_POINT('Ctrl Pts',(-18.1487418746945,-1.94912136870076,
0.46991636905064));
#30366=CARTESIAN_POINT('Ctrl Pts',(-18.1218696921242,-1.95320927907148,
-0.00174204714352619));
#30367=CARTESIAN_POINT('Origin',(-9.8,0.,0.));
#30368=CARTESIAN_POINT('',(-17.3201303078758,-1.95716036932443,0.000219777629121352));
#30369=CARTESIAN_POINT('',(-17.4218696921242,-1.95710975664994,0.000358848027250084));
#30370=CARTESIAN_POINT('',(-9.8,-1.954,-2.39295984553393E-16));
#30371=CARTESIAN_POINT('Ctrl Pts',(-17.3201303078758,-1.95716036932443,
0.000219777629121352));
#30372=CARTESIAN_POINT('Ctrl Pts',(-17.3208085792439,-1.95717926909536,
0.0120624621000906));
#30373=CARTESIAN_POINT('Ctrl Pts',(-17.321486850612,-1.95708105723414,0.0239048246808731));
#30374=CARTESIAN_POINT('Ctrl Pts',(-17.3221651219801,-1.95686477834934,
0.0357450305932741));
#30375=CARTESIAN_POINT('Ctrl Pts',(-17.3591782953177,-1.94506246996874,
0.68186340501921));
#30376=CARTESIAN_POINT('Ctrl Pts',(-17.3961914686552,-1.58167196389125,
1.32155950228172));
#30377=CARTESIAN_POINT('Ctrl Pts',(-17.4332046419928,-1.03273148765314,
1.66254718585494));
#30378=CARTESIAN_POINT('Ctrl Pts',(-17.4702178153304,-0.483791011415034,
2.00353486942816));
#30379=CARTESIAN_POINT('Ctrl Pts',(-17.507230988668,0.250699434983697,2.04581413931209));
#30380=CARTESIAN_POINT('Ctrl Pts',(-17.5442441620055,0.835140850126002,
1.77006701011294));
#30381=CARTESIAN_POINT('Ctrl Pts',(-17.5812573353431,1.41958226526831,1.4943198809138));
#30382=CARTESIAN_POINT('Ctrl Pts',(-17.6182705086806,1.85397464915419,0.900546352631588));
#30383=CARTESIAN_POINT('Ctrl Pts',(-17.6552836820182,1.93983801723647,0.260049878109278));
#30384=CARTESIAN_POINT('Ctrl Pts',(-17.6922968553558,2.02570138531875,-0.380446596413026));
#30385=CARTESIAN_POINT('Ctrl Pts',(-17.7293100286933,1.76303573759744,-1.06766601717542));
#30386=CARTESIAN_POINT('Ctrl Pts',(-17.7663232020309,1.27185670261682,-1.48760815212437));
#30387=CARTESIAN_POINT('Ctrl Pts',(-17.8033363753685,0.780677667636197,
-1.90755028707332));
#30388=CARTESIAN_POINT('Ctrl Pts',(-17.840349548706,0.0609852453962589,
-2.06021513620881));
#30389=CARTESIAN_POINT('Ctrl Pts',(-17.8773627220436,-0.558382994856356,
-1.875848033151));
#30390=CARTESIAN_POINT('Ctrl Pts',(-17.9143758953811,-1.17775123510897,
-1.69148093009319));
#30391=CARTESIAN_POINT('Ctrl Pts',(-17.9513890687187,-1.69679529337426,
-1.17008187484208));
#30392=CARTESIAN_POINT('Ctrl Pts',(-17.9884022420563,-1.87835663251658,
-0.54988532920897));
#30393=CARTESIAN_POINT('Ctrl Pts',(-17.9989782639961,-1.93023537008609,
-0.372672416017184));
#30394=CARTESIAN_POINT('Ctrl Pts',(-18.0095542859359,-1.95456017557276,
-0.187393136206644));
#30395=CARTESIAN_POINT('Ctrl Pts',(-18.0201303078758,-1.95299307732975,
-0.00171153559867271));
#30396=CARTESIAN_POINT('Ctrl Pts',(-18.1218696921242,-1.95320927907148,
-0.00174204714352619));
#30397=CARTESIAN_POINT('Ctrl Pts',(-18.1117287013569,-1.95475196959239,
-0.179735912414574));
#30398=CARTESIAN_POINT('Ctrl Pts',(-18.1015877105896,-1.93242005916289,
-0.357349664660824));
#30399=CARTESIAN_POINT('Ctrl Pts',(-18.0914467198223,-1.88466923704063,
-0.527844244331786));
#30400=CARTESIAN_POINT('Ctrl Pts',(-18.0544335464847,-1.71038553076609,
-1.15012520043117));
#30401=CARTESIAN_POINT('Ctrl Pts',(-18.0174203731472,-1.19748477603389,
-1.67756837456562));
#30402=CARTESIAN_POINT('Ctrl Pts',(-17.9804071998096,-0.580318741193403,
-1.86917817188516));
#30403=CARTESIAN_POINT('Ctrl Pts',(-17.943394026472,0.0368472936470773,
-2.0607879692047));
#30404=CARTESIAN_POINT('Ctrl Pts',(-17.9063808531345,0.758278608595835,
-1.91656438970933));
#30405=CARTESIAN_POINT('Ctrl Pts',(-17.8693676797969,1.25434321128846,-1.50240489715304));
#30406=CARTESIAN_POINT('Ctrl Pts',(-17.8323545064593,1.75040781398108,-1.08824540459674));
#30407=CARTESIAN_POINT('Ctrl Pts',(-17.7953413331218,2.02110570441758,-0.404149998979508));
#30408=CARTESIAN_POINT('Ctrl Pts',(-17.7583281597842,1.94275115623478,0.237308353210707));
#30409=CARTESIAN_POINT('Ctrl Pts',(-17.7213149864467,1.86439660805198,0.878766705400926));
#30410=CARTESIAN_POINT('Ctrl Pts',(-17.6843018131091,1.43698962124989,1.47758800416414));
#30411=CARTESIAN_POINT('Ctrl Pts',(-17.6472886397715,0.855818482331675,
1.7601624734435));
#30412=CARTESIAN_POINT('Ctrl Pts',(-17.610275466434,0.274647343413464,2.04273694272287));
#30413=CARTESIAN_POINT('Ctrl Pts',(-17.5732622930964,-0.460287947620861,
2.00906458251839));
#30414=CARTESIAN_POINT('Ctrl Pts',(-17.5362491197588,-1.01318514831372,
1.6745307213773));
#30415=CARTESIAN_POINT('Ctrl Pts',(-17.4992359464213,-1.56608234900657,
1.33999686023621));
#30416=CARTESIAN_POINT('Ctrl Pts',(-17.4622227730837,-1.93694145935795,
0.704601498158489));
#30417=CARTESIAN_POINT('Ctrl Pts',(-17.4252095997461,-1.9563117338864,0.0586657258015617));
#30418=CARTESIAN_POINT('Ctrl Pts',(-17.4240962972055,-1.95689436363416,
0.0392369151482447));
#30419=CARTESIAN_POINT('Ctrl Pts',(-17.4229829946649,-1.95715899471935,
0.0197985683844457));
#30420=CARTESIAN_POINT('Ctrl Pts',(-17.4218696921242,-1.95710975664994,
0.000358848027250084));
#30421=CARTESIAN_POINT('Origin',(-9.8,0.,0.));
#30422=CARTESIAN_POINT('',(-16.6201303078758,-1.95236106975453,0.00156080202577326));
#30423=CARTESIAN_POINT('',(-16.7218696921242,-1.95217490710565,0.00149575073417193));
#30424=CARTESIAN_POINT('',(-9.8,-1.954,-2.39295984553393E-16));
#30425=CARTESIAN_POINT('Ctrl Pts',(-16.6201303078758,-1.95236106975453,
0.00156080202577326));
#30426=CARTESIAN_POINT('Ctrl Pts',(-16.6320628725518,-1.95393611722315,
0.211230577376388));
#30427=CARTESIAN_POINT('Ctrl Pts',(-16.6439954372279,-1.92281737418396,
0.420445287656267));
#30428=CARTESIAN_POINT('Ctrl Pts',(-16.655928001904,-1.85702132802313,0.618117508955001));
#30429=CARTESIAN_POINT('Ctrl Pts',(-16.6929411752415,-1.65293104839012,
1.23126953365152));
#30430=CARTESIAN_POINT('Ctrl Pts',(-16.7299543485791,-1.11519135743181,
1.73336492166902));
#30431=CARTESIAN_POINT('Ctrl Pts',(-16.7669675219167,-0.489503073786642,
1.89498923702786));
#30432=CARTESIAN_POINT('Ctrl Pts',(-16.8039806952542,0.136185209858534,
2.0566135523867));
#30433=CARTESIAN_POINT('Ctrl Pts',(-16.8409938685918,0.849822086190574,
1.87776679508686));
#30434=CARTESIAN_POINT('Ctrl Pts',(-16.8780070419294,1.32533684172017,1.44016656101051));
#30435=CARTESIAN_POINT('Ctrl Pts',(-16.9150202152669,1.80085159724978,1.00256632693417));
#30436=CARTESIAN_POINT('Ctrl Pts',(-16.9520333886045,2.03824423197693,0.306212616081319));
#30437=CARTESIAN_POINT('Ctrl Pts',(-16.989046561942,1.92904671630549,-0.330720779401667));
#30438=CARTESIAN_POINT('Ctrl Pts',(-17.0260597352796,1.81984920063405,-0.96765417488465));
#30439=CARTESIAN_POINT('Ctrl Pts',(-17.0630729086172,1.36406153456402,-1.54516725499777));
#30440=CARTESIAN_POINT('Ctrl Pts',(-17.1000860819547,0.769939505430447,
-1.79938618037108));
#30441=CARTESIAN_POINT('Ctrl Pts',(-17.1370992552923,0.175817476296884,
-2.05360510574439));
#30442=CARTESIAN_POINT('Ctrl Pts',(-17.1741124286299,-0.556638915900209,
-1.9845298763779));
#30443=CARTESIAN_POINT('Ctrl Pts',(-17.2111256019674,-1.09276005665691,
-1.62372193589998));
#30444=CARTESIAN_POINT('Ctrl Pts',(-17.2474605039369,-1.61905670556847,
-1.26952584934724));
#30445=CARTESIAN_POINT('Ctrl Pts',(-17.2837954059063,-1.95614791124902,
-0.634191166918971));
#30446=CARTESIAN_POINT('Ctrl Pts',(-17.3201303078758,-1.95716036932443,
0.000219777629121352));
#30447=CARTESIAN_POINT('Ctrl Pts',(-17.4218696921242,-1.95710975664994,
0.000358848027250084));
#30448=CARTESIAN_POINT('Ctrl Pts',(-17.3859698213273,-1.95552201184067,
-0.626499911094741));
#30449=CARTESIAN_POINT('Ctrl Pts',(-17.3500699505304,-1.62756593762931,
-1.25478696406307));
#30450=CARTESIAN_POINT('Ctrl Pts',(-17.3141700797335,-1.11170569044781,
-1.61080964516247));
#30451=CARTESIAN_POINT('Ctrl Pts',(-17.2771569063959,-0.579847933775247,
-1.97787306113345));
#30452=CARTESIAN_POINT('Ctrl Pts',(-17.2401437330583,0.151749018275395,
-2.05552371043926));
#30453=CARTESIAN_POINT('Ctrl Pts',(-17.2031305597207,0.748808243613774,
-1.80828191396906));
#30454=CARTESIAN_POINT('Ctrl Pts',(-17.1661173863832,1.34586746895216,-1.56104011749885));
#30455=CARTESIAN_POINT('Ctrl Pts',(-17.1291042130456,1.80838896757828,-0.988905875252619));
#30456=CARTESIAN_POINT('Ctrl Pts',(-17.0920910397081,1.92504016834594,-0.353295362990227));
#30457=CARTESIAN_POINT('Ctrl Pts',(-17.0550778663705,2.04169136911361,0.282315149272168));
#30458=CARTESIAN_POINT('Ctrl Pts',(-17.0180646930329,1.81247227202281,0.981401931550726));
#30459=CARTESIAN_POINT('Ctrl Pts',(-16.9810515196954,1.34211630309758,1.42454241453319));
#30460=CARTESIAN_POINT('Ctrl Pts',(-16.9440383463578,0.871760334172357,
1.86768289751565));
#30461=CARTESIAN_POINT('Ctrl Pts',(-16.9070251730202,0.160267493412704,
2.05487708120202));
#30462=CARTESIAN_POINT('Ctrl Pts',(-16.8700119996827,-0.467271145973578,
1.9005933125143));
#30463=CARTESIAN_POINT('Ctrl Pts',(-16.8329988263451,-1.09480978535987,
1.74630954382658));
#30464=CARTESIAN_POINT('Ctrl Pts',(-16.7959856530075,-1.63839422337278,
1.25054782276476));
#30465=CARTESIAN_POINT('Ctrl Pts',(-16.75897247967,-1.84965309417818,0.639828644336359));
#30466=CARTESIAN_POINT('Ctrl Pts',(-16.7466048838214,-1.92024321380182,
0.435762705247683));
#30467=CARTESIAN_POINT('Ctrl Pts',(-16.7342372879728,-1.95372925218912,
0.218861789684893));
#30468=CARTESIAN_POINT('Ctrl Pts',(-16.7218696921242,-1.95217490710565,
0.00149575073417193));
#30469=CARTESIAN_POINT('Origin',(-9.8,0.,0.));
#30470=CARTESIAN_POINT('',(-15.9201303078758,-1.9516232757602,-0.00122528121799068));
#30471=CARTESIAN_POINT('',(-16.0218696921242,-1.951775199121,-0.00131382171386765));
#30472=CARTESIAN_POINT('',(-9.8,-1.954,-2.39295984553393E-16));
#30473=CARTESIAN_POINT('Ctrl Pts',(-15.9201303078758,-1.9516232757602,-0.00122528121799068));
#30474=CARTESIAN_POINT('Ctrl Pts',(-15.9433171658598,-1.94927914488889,
0.406583857041756));
#30475=CARTESIAN_POINT('Ctrl Pts',(-15.9665040238438,-1.82458420503018,
0.81570542027797));
#30476=CARTESIAN_POINT('Ctrl Pts',(-15.9896908818278,-1.58792615951522,
1.14415382687092));
#30477=CARTESIAN_POINT('Ctrl Pts',(-16.0267040551654,-1.21014900374817,
1.66845590411029));
#30478=CARTESIAN_POINT('Ctrl Pts',(-16.0637172285029,-0.547070532187443,
1.98718885565735));
#30479=CARTESIAN_POINT('Ctrl Pts',(-16.1007304018405,0.0983393870045533,
1.95471911859019));
#30480=CARTESIAN_POINT('Ctrl Pts',(-16.1377435751781,0.743749306196545,
1.92224938152302));
#30481=CARTESIAN_POINT('Ctrl Pts',(-16.1747567485156,1.37149067301981,1.53857695584164));
#30482=CARTESIAN_POINT('Ctrl Pts',(-16.2117699218532,1.69473963886053,0.979007162429953));
#30483=CARTESIAN_POINT('Ctrl Pts',(-16.2487830951907,2.01798860470126,0.41943736901826));
#30484=CARTESIAN_POINT('Ctrl Pts',(-16.2857962685283,2.03674516955944,-0.316029792123737));
#30485=CARTESIAN_POINT('Ctrl Pts',(-16.3228094418659,1.74243919547003,-0.89134904369965));
#30486=CARTESIAN_POINT('Ctrl Pts',(-16.3598226152035,1.44813322138062,-1.46666829527556));
#30487=CARTESIAN_POINT('Ctrl Pts',(-16.396835788541,0.840764708343617,-1.88183963728539));
#30488=CARTESIAN_POINT('Ctrl Pts',(-16.4338489618786,0.197848861895412,
-1.94716545148987));
#30489=CARTESIAN_POINT('Ctrl Pts',(-16.4708621352161,-0.445066984552789,
-2.01249126569435));
#30490=CARTESIAN_POINT('Ctrl Pts',(-16.5078753085537,-1.12353016441219,
-1.72797155209348));
#30491=CARTESIAN_POINT('Ctrl Pts',(-16.5448884818913,-1.52754132018803,
-1.22360736460528));
#30492=CARTESIAN_POINT('Ctrl Pts',(-16.5699690905528,-1.8013045449859,-0.881843617576629));
#30493=CARTESIAN_POINT('Ctrl Pts',(-16.5950496992143,-1.94905053675042,
-0.439136208756951));
#30494=CARTESIAN_POINT('Ctrl Pts',(-16.6201303078758,-1.95236106975453,
0.00156080202577326));
#30495=CARTESIAN_POINT('Ctrl Pts',(-16.7218696921242,-1.95217490710565,
0.00149575073417193));
#30496=CARTESIAN_POINT('Ctrl Pts',(-16.6972241146353,-1.94907747954834,
-0.431661317302269));
#30497=CARTESIAN_POINT('Ctrl Pts',(-16.6725785371463,-1.80683227309339,
-0.866665422383789));
#30498=CARTESIAN_POINT('Ctrl Pts',(-16.6479329596573,-1.54177007931888,
-1.20562941457546));
#30499=CARTESIAN_POINT('Ctrl Pts',(-16.6109197863197,-1.14369489005632,
-1.71469165926392));
#30500=CARTESIAN_POINT('Ctrl Pts',(-16.5739066129822,-0.468611207933312,
-2.00713951284586));
#30501=CARTESIAN_POINT('Ctrl Pts',(-16.5368934396446,0.175025749589254,
-1.9493494427573));
#30502=CARTESIAN_POINT('Ctrl Pts',(-16.499880266307,0.818662707111826,-1.89155937266874));
#30503=CARTESIAN_POINT('Ctrl Pts',(-16.4628670929695,1.43085294003395,-1.48353137890967));
#30504=CARTESIAN_POINT('Ctrl Pts',(-16.4258539196319,1.73187813124758,-0.91169918362098));
#30505=CARTESIAN_POINT('Ctrl Pts',(-16.3888407462943,2.0329033224612,-0.33986698833229));
#30506=CARTESIAN_POINT('Ctrl Pts',(-16.3518275729568,2.02276347196631,0.395769408486024));
#30507=CARTESIAN_POINT('Ctrl Pts',(-16.3148143996192,1.70609161990569,0.959087403412657));
#30508=CARTESIAN_POINT('Ctrl Pts',(-16.2778012262816,1.38941976784508,1.52240539833928));
#30509=CARTESIAN_POINT('Ctrl Pts',(-16.2407880529441,0.766215914218737,
1.91340499137424));
#30510=CARTESIAN_POINT('Ctrl Pts',(-16.2037748796065,0.121230654114145,
1.95343297592505));
#30511=CARTESIAN_POINT('Ctrl Pts',(-16.166761706269,-0.523754605990456,
1.99346096047586));
#30512=CARTESIAN_POINT('Ctrl Pts',(-16.1297485329314,-1.19052127257331,
1.68251733654252));
#30513=CARTESIAN_POINT('Ctrl Pts',(-16.0927353595938,-1.57441428935352,
1.1626766138498));
#30514=CARTESIAN_POINT('Ctrl Pts',(-16.0691134704373,-1.81941566244965,
0.830913113905955));
#30515=CARTESIAN_POINT('Ctrl Pts',(-16.0454915812807,-1.94920201372017,
0.41406539417118));
#30516=CARTESIAN_POINT('Ctrl Pts',(-16.0218696921242,-1.951775199121,-0.00131382171386765));
#30517=CARTESIAN_POINT('Origin',(-9.8,0.,0.));
#30518=CARTESIAN_POINT('',(-15.2201303078758,-1.95678697592279,-0.000800724488720095));
#30519=CARTESIAN_POINT('',(-15.3218696921242,-1.95690589693301,-0.000674027605478421));
#30520=CARTESIAN_POINT('',(-9.8,-1.954,-2.39295984553393E-16));
#30521=CARTESIAN_POINT('Ctrl Pts',(-15.2201303078758,-1.95678697592279,
-0.000800724488720095));
#30522=CARTESIAN_POINT('Ctrl Pts',(-15.2545714591677,-1.95366270876428,
0.600851523163264));
#30523=CARTESIAN_POINT('Ctrl Pts',(-15.2890126104597,-1.65520957823559,
1.20518249057995));
#30524=CARTESIAN_POINT('Ctrl Pts',(-15.3234537617516,-1.17410501132559,
1.56591024327599));
#30525=CARTESIAN_POINT('Ctrl Pts',(-15.3604669350892,-0.657072157877076,
1.95357669278071));
#30526=CARTESIAN_POINT('Ctrl Pts',(-15.3974801084268,0.0709111245972353,
2.05989740706708));
#30527=CARTESIAN_POINT('Ctrl Pts',(-15.4344932817643,0.677219048087142,
1.83629295825163));
#30528=CARTESIAN_POINT('Ctrl Pts',(-15.4715064551019,1.28352697157704,1.61268850943619));
#30529=CARTESIAN_POINT('Ctrl Pts',(-15.5085196284395,1.76815953608255,1.05915889751893));
#30530=CARTESIAN_POINT('Ctrl Pts',(-15.545532801777,1.90968131507004,0.428619577818016));
#30531=CARTESIAN_POINT('Ctrl Pts',(-15.5825459751146,2.05120309405753,-0.201919741882898));
#30532=CARTESIAN_POINT('Ctrl Pts',(-15.6195591484522,1.84961408752702,-0.909468769367463));
#30533=CARTESIAN_POINT('Ctrl Pts',(-15.6565723217897,1.39702314435684,-1.37073841477789));
#30534=CARTESIAN_POINT('Ctrl Pts',(-15.6935854951273,0.944432201186666,
-1.83200806018831));
#30535=CARTESIAN_POINT('Ctrl Pts',(-15.7305986684648,0.240839321376827,
-2.0469983235246));
#30536=CARTESIAN_POINT('Ctrl Pts',(-15.7676118418024,-0.392274024660755,
-1.91747713342123));
#30537=CARTESIAN_POINT('Ctrl Pts',(-15.80462501514,-1.02538737069834,-1.78795594331785));
#30538=CARTESIAN_POINT('Ctrl Pts',(-15.8416381884775,-1.58802118296367,
-1.31392329977481));
#30539=CARTESIAN_POINT('Ctrl Pts',(-15.8786513618151,-1.82310016910965,
-0.71197137653746));
#30540=CARTESIAN_POINT('Ctrl Pts',(-15.8924776771687,-1.91091420671742,
-0.487111512660019));
#30541=CARTESIAN_POINT('Ctrl Pts',(-15.9063039925222,-1.95302108018369,
-0.244401728562753));
#30542=CARTESIAN_POINT('Ctrl Pts',(-15.9201303078758,-1.9516232757602,-0.00122528121799068));
#30543=CARTESIAN_POINT('Ctrl Pts',(-16.0218696921242,-1.951775199121,-0.00131382171386765));
#30544=CARTESIAN_POINT('Ctrl Pts',(-16.0084784079432,-1.95323394176112,
-0.236792918493611));
#30545=CARTESIAN_POINT('Ctrl Pts',(-15.9950871237622,-1.91380926057871,
-0.471800071470502));
#30546=CARTESIAN_POINT('Ctrl Pts',(-15.9816958395811,-1.8313152224601,-0.690566303043669));
#30547=CARTESIAN_POINT('Ctrl Pts',(-15.9446826662436,-1.60330377180891,
-1.29523067579235));
#30548=CARTESIAN_POINT('Ctrl Pts',(-15.907669492906,-1.04626150352895,-1.77582159983761));
#30549=CARTESIAN_POINT('Ctrl Pts',(-15.8706563195684,-0.414708854972982,
-1.91275033094355));
#30550=CARTESIAN_POINT('Ctrl Pts',(-15.8336431462309,0.216843793582987,
-2.0496790620495));
#30551=CARTESIAN_POINT('Ctrl Pts',(-15.7966299728933,0.922906822414965,
-1.84294560021614));
#30552=CARTESIAN_POINT('Ctrl Pts',(-15.7596167995557,1.38087011532323,-1.38700936821731));
#30553=CARTESIAN_POINT('Ctrl Pts',(-15.7226036262182,1.83883340823148,-0.931073136218487));
#30554=CARTESIAN_POINT('Ctrl Pts',(-15.6855904528806,2.04869696521603,-0.225934134054202));
#30555=CARTESIAN_POINT('Ctrl Pts',(-15.648577279543,1.9145711790607,0.406219722841795));
#30556=CARTESIAN_POINT('Ctrl Pts',(-15.6115641062055,1.78044539290536,1.0383735797378));
#30557=CARTESIAN_POINT('Ctrl Pts',(-15.5745509328679,1.30233026361014,1.59754229136552));
#30558=CARTESIAN_POINT('Ctrl Pts',(-15.5375377595304,0.698683310008129,
1.82823381853421));
#30559=CARTESIAN_POINT('Ctrl Pts',(-15.5005245861928,0.0950363564061148,
2.05892534570289));
#30560=CARTESIAN_POINT('Ctrl Pts',(-15.4635114128552,-0.634142421502691,
1.96113968841256));
#30561=CARTESIAN_POINT('Ctrl Pts',(-15.4264982395177,-1.15568099705043,
1.5795564871103));
#30562=CARTESIAN_POINT('Ctrl Pts',(-15.3916220570532,-1.64710804539289,
1.22000435596431));
#30563=CARTESIAN_POINT('Ctrl Pts',(-15.3567458745887,-1.95417934548115,
0.608479302503191));
#30564=CARTESIAN_POINT('Ctrl Pts',(-15.3218696921242,-1.95690589693301,
-0.000674027605478421));
#30565=CARTESIAN_POINT('Origin',(-9.8,0.,0.));
#30566=CARTESIAN_POINT('',(-14.5201303078758,-1.95396550297987,0.00177712178281789));
#30567=CARTESIAN_POINT('',(-14.6218696921242,-1.95373627769492,0.00177775396232179));
#30568=CARTESIAN_POINT('',(-9.8,-1.954,-2.39295984553393E-16));
#30569=CARTESIAN_POINT('Ctrl Pts',(-14.5201303078758,-1.95396550297987,
0.00177712178281789));
#30570=CARTESIAN_POINT('Ctrl Pts',(-14.5288125791381,-1.95535803437996,
0.154017333838736));
#30571=CARTESIAN_POINT('Ctrl Pts',(-14.5374948504005,-1.93906235797112,
0.305962769432957));
#30572=CARTESIAN_POINT('Ctrl Pts',(-14.5461771216628,-1.90394399117853,
0.453425568392138));
#30573=CARTESIAN_POINT('Ctrl Pts',(-14.5831902950004,-1.75423176057083,
1.08207053625807));
#30574=CARTESIAN_POINT('Ctrl Pts',(-14.6202034683379,-1.26243956445243,
1.62924892552931));
#30575=CARTESIAN_POINT('Ctrl Pts',(-14.6572166416755,-0.65327416561486,
1.84494724373267));
#30576=CARTESIAN_POINT('Ctrl Pts',(-14.6942298150131,-0.0441087667772883,
2.06064556193603));
#30577=CARTESIAN_POINT('Ctrl Pts',(-14.7312429883506,0.682429834779477,
1.9448638090715));
#30578=CARTESIAN_POINT('Ctrl Pts',(-14.7682561616882,1.1943759460504,1.55050429445157));
#30579=CARTESIAN_POINT('Ctrl Pts',(-14.8052693350257,1.70632205732133,1.15614477983164));
#30580=CARTESIAN_POINT('Ctrl Pts',(-14.8422825083633,2.00367567830644,0.48320750345631));
#30581=CARTESIAN_POINT('Ctrl Pts',(-14.8792956817009,1.95057176254247,-0.160833040102267));
#30582=CARTESIAN_POINT('Ctrl Pts',(-14.9163088550384,1.89746784677849,-0.804873583660848));
#30583=CARTESIAN_POINT('Ctrl Pts',(-14.953322028376,1.49390639426542,-1.42001739440267));
#30584=CARTESIAN_POINT('Ctrl Pts',(-14.9903352017136,0.924280301631946,
-1.72519662404948));
#30585=CARTESIAN_POINT('Ctrl Pts',(-15.0273483750511,0.35465420899847,-2.03037585369629));
#30586=CARTESIAN_POINT('Ctrl Pts',(-15.0643615483887,-0.381036523755413,
-2.02559050224809));
#30587=CARTESIAN_POINT('Ctrl Pts',(-15.1013747217263,-0.946644466317395,
-1.71302706400314));
#30588=CARTESIAN_POINT('Ctrl Pts',(-15.1383878950638,-1.51225240887937,
-1.4004636257582));
#30589=CARTESIAN_POINT('Ctrl Pts',(-15.1754010684014,-1.90777756124945,
-0.780122100716514));
#30590=CARTESIAN_POINT('Ctrl Pts',(-15.212414241739,-1.95249892522313,-0.135445245834147));
#30591=CARTESIAN_POINT('Ctrl Pts',(-15.2149862637846,-1.95560658456919,
-0.0906470582287079));
#30592=CARTESIAN_POINT('Ctrl Pts',(-15.2175582858302,-1.95702029228147,
-0.045731360855399));
#30593=CARTESIAN_POINT('Ctrl Pts',(-15.2201303078758,-1.95678697592279,
-0.000800724488720095));
#30594=CARTESIAN_POINT('Ctrl Pts',(-15.3218696921242,-1.95690589693301,
-0.000674027605478421));
#30595=CARTESIAN_POINT('Ctrl Pts',(-15.3197327012511,-1.95707296268264,
-0.0379990733749708));
#30596=CARTESIAN_POINT('Ctrl Pts',(-15.3175957103781,-1.95609737832443,
-0.0753152146046056));
#30597=CARTESIAN_POINT('Ctrl Pts',(-15.315458719505,-1.95395154045615,-0.112563939451326));
#30598=CARTESIAN_POINT('Ctrl Pts',(-15.2784455461674,-1.91678513512746,
-0.75772041939657));
#30599=CARTESIAN_POINT('Ctrl Pts',(-15.2414323728298,-1.52855395128338,
-1.38265263397289));
#30600=CARTESIAN_POINT('Ctrl Pts',(-15.2044191994923,-0.96664627044783,
-1.70182027568869));
#30601=CARTESIAN_POINT('Ctrl Pts',(-15.1674060261547,-0.404738589612277,
-2.0209879174045));
#30602=CARTESIAN_POINT('Ctrl Pts',(-15.1303928528172,0.330845588214744,
-2.03439098625978));
#30603=CARTESIAN_POINT('Ctrl Pts',(-15.0933796794796,0.904007519163827,
-1.73590543181679));
#30604=CARTESIAN_POINT('Ctrl Pts',(-15.056366506142,1.4771694501129,-1.43741987737381));
#30605=CARTESIAN_POINT('Ctrl Pts',(-15.0193533328045,1.88790913418403,-0.827045699632558));
#30606=CARTESIAN_POINT('Ctrl Pts',(-14.9823401594669,1.94855383991442,-0.183671434552528));
#30607=CARTESIAN_POINT('Ctrl Pts',(-14.9453269861293,2.0091985456448,0.459702830527515));
#30608=CARTESIAN_POINT('Ctrl Pts',(-14.9083138127918,1.71974827303444,1.13607718294633));
#30609=CARTESIAN_POINT('Ctrl Pts',(-14.8713006394542,1.21245691765294,1.53640667980563));
#30610=CARTESIAN_POINT('Ctrl Pts',(-14.8342874661166,0.705165562271449,
1.93673617666491));
#30611=CARTESIAN_POINT('Ctrl Pts',(-14.7972742927791,-0.0199668758811834,
2.06102081796467));
#30612=CARTESIAN_POINT('Ctrl Pts',(-14.7602611194415,-0.631617199612173,
1.85247320522319));
#30613=CARTESIAN_POINT('Ctrl Pts',(-14.7232479461039,-1.24326752334318,
1.64392559248171));
#30614=CARTESIAN_POINT('Ctrl Pts',(-14.6862347727664,-1.74143573265255,
1.10254572569898));
#30615=CARTESIAN_POINT('Ctrl Pts',(-14.6492215994288,-1.89850177475563,
0.475697670969221));
#30616=CARTESIAN_POINT('Ctrl Pts',(-14.640104296994,-1.93719120554397,0.321288773262618));
#30617=CARTESIAN_POINT('Ctrl Pts',(-14.6309869945591,-1.95518377170558,
0.161693970317362));
#30618=CARTESIAN_POINT('Ctrl Pts',(-14.6218696921242,-1.95373627769492,
0.00177775396232179));
#30619=CARTESIAN_POINT('Origin',(-9.8,0.,0.));
#30620=CARTESIAN_POINT('',(-13.8201303078758,-1.95088537187799,-0.000408160563786925));
#30621=CARTESIAN_POINT('',(-13.9218696921242,-1.95094021917743,-0.000529095196661905));
#30622=CARTESIAN_POINT('',(-9.8,-1.954,-2.39295984553393E-16));
#30623=CARTESIAN_POINT('Ctrl Pts',(-13.8201303078758,-1.95088537187799,
-0.000408160563786925));
#30624=CARTESIAN_POINT('Ctrl Pts',(-13.8400668724461,-1.95022879632092,
0.350567026998221));
#30625=CARTESIAN_POINT('Ctrl Pts',(-13.8600034370163,-1.85987981718048,
0.701857479589949));
#30626=CARTESIAN_POINT('Ctrl Pts',(-13.8799400015866,-1.68186073672999,
1.00097049400201));
#30627=CARTESIAN_POINT('Ctrl Pts',(-13.9169531749242,-1.35135990952491,
1.55628792649757));
#30628=CARTESIAN_POINT('Ctrl Pts',(-13.9539663482618,-0.718680622512158,
1.93176185852677));
#30629=CARTESIAN_POINT('Ctrl Pts',(-13.9909795215993,-0.0729029294054372,
1.95583297612569));
#30630=CARTESIAN_POINT('Ctrl Pts',(-14.0279926949369,0.572874763701284,
1.97990409372461));
#30631=CARTESIAN_POINT('Ctrl Pts',(-14.0650058682745,1.23175086290198,1.65257239689324));
#30632=CARTESIAN_POINT('Ctrl Pts',(-14.102019041612,1.60267562299808,1.12340033606203));
#30633=CARTESIAN_POINT('Ctrl Pts',(-14.1390322149496,1.97360038309417,0.594228275230817));
#30634=CARTESIAN_POINT('Ctrl Pts',(-14.1760453882871,2.05657380408567,-0.136784149600244));
#30635=CARTESIAN_POINT('Ctrl Pts',(-14.2130585616247,1.81368416436353,-0.735627092726691));
#30636=CARTESIAN_POINT('Ctrl Pts',(-14.2500717349623,1.57079452464139,-1.33447003585314));
#30637=CARTESIAN_POINT('Ctrl Pts',(-14.2870849082998,1.00204182420563,-1.80114349727497));
#30638=CARTESIAN_POINT('Ctrl Pts',(-14.3240980816374,0.367297161362722,
-1.9224178169356));
#30639=CARTESIAN_POINT('Ctrl Pts',(-14.361111254975,-0.267447501480182,
-2.04369213659623));
#30640=CARTESIAN_POINT('Ctrl Pts',(-14.3981244283125,-0.968184126730219,
-1.81956731449565));
#30641=CARTESIAN_POINT('Ctrl Pts',(-14.4351376016501,-1.41473630680673,
-1.35244913021504));
#30642=CARTESIAN_POINT('Ctrl Pts',(-14.4634685037253,-1.75653964179354,
-0.994904009300521));
#30643=CARTESIAN_POINT('Ctrl Pts',(-14.4917994058005,-1.94942156861746,
-0.494994104241234));
#30644=CARTESIAN_POINT('Ctrl Pts',(-14.5201303078758,-1.95396550297987,
0.00177712178281789));
#30645=CARTESIAN_POINT('Ctrl Pts',(-14.6218696921242,-1.95373627769492,
0.00177775396232179));
#30646=CARTESIAN_POINT('Ctrl Pts',(-14.5939738212215,-1.94930743414802,
-0.487511940940269));
#30647=CARTESIAN_POINT('Ctrl Pts',(-14.5660779503188,-1.76288976123999,
-0.979810559152193));
#30648=CARTESIAN_POINT('Ctrl Pts',(-14.5381820794161,-1.43048209022845,
-1.3357837596151));
#30649=CARTESIAN_POINT('Ctrl Pts',(-14.5011689060785,-0.989432488701429,
-1.80810089279285));
#30650=CARTESIAN_POINT('Ctrl Pts',(-14.464155732741,-0.291369410750597,
-2.04041891647158));
#30651=CARTESIAN_POINT('Ctrl Pts',(-14.4271425594034,0.34475231736069,-1.92658846217614));
#30652=CARTESIAN_POINT('Ctrl Pts',(-14.3901293860659,0.980874045471991,
-1.8127580078807));
#30653=CARTESIAN_POINT('Ctrl Pts',(-14.3531162127283,1.55505442374375,-1.3527790756111));
#30654=CARTESIAN_POINT('Ctrl Pts',(-14.3161030393907,1.80494237162162,-0.756822501013755));
#30655=CARTESIAN_POINT('Ctrl Pts',(-14.2790898660532,2.0548303194995,-0.160865926416412));
#30656=CARTESIAN_POINT('Ctrl Pts',(-14.2420766927156,1.98042583698348,0.571068290508656));
#30657=CARTESIAN_POINT('Ctrl Pts',(-14.205063519378,1.61572537732216,1.10454912430049));
#30658=CARTESIAN_POINT('Ctrl Pts',(-14.1680503460405,1.25102491766083,1.63802995809231));
#30659=CARTESIAN_POINT('Ctrl Pts',(-14.1310371727029,0.596028480854202,
1.9730574087509));
#30660=CARTESIAN_POINT('Ctrl Pts',(-14.0940239993653,-0.0499868601460479,
1.9565527278171));
#30661=CARTESIAN_POINT('Ctrl Pts',(-14.0570108260278,-0.696002201146311,
1.9400480468833));
#30662=CARTESIAN_POINT('Ctrl Pts',(-14.0199976526902,-1.33303644634019,
1.57201123435709));
#30663=CARTESIAN_POINT('Ctrl Pts',(-13.9829844793526,-1.67001970044536,
1.02060347982955));
#30664=CARTESIAN_POINT('Ctrl Pts',(-13.9626128836098,-1.85549114225117,
0.717115428096236));
#30665=CARTESIAN_POINT('Ctrl Pts',(-13.942241287867,-1.95006914783739,0.358079434458608));
#30666=CARTESIAN_POINT('Ctrl Pts',(-13.9218696921242,-1.95094021917743,
-0.000529095196661905));
#30667=CARTESIAN_POINT('Origin',(-9.8,0.,0.));
#30668=CARTESIAN_POINT('',(-13.1201303078758,-1.95545730741116,-0.00153438558903124));
#30669=CARTESIAN_POINT('',(-13.2218696921242,-1.95566871115984,-0.00146207300122905));
#30670=CARTESIAN_POINT('',(-9.8,-1.954,-2.39295984553393E-16));
#30671=CARTESIAN_POINT('Ctrl Pts',(-13.1201303078758,-1.95545730741116,
-0.00153438558903124));
#30672=CARTESIAN_POINT('Ctrl Pts',(-13.151321165754,-1.95075080529458,0.544310729119318));
#30673=CARTESIAN_POINT('Ctrl Pts',(-13.1825120236322,-1.7119678003024,1.09376537173191));
#30674=CARTESIAN_POINT('Ctrl Pts',(-13.2137028815105,-1.30649016387798,
1.45728546253184));
#30675=CARTESIAN_POINT('Ctrl Pts',(-13.250716054848,-0.825323082803425,
1.88866289321973));
#30676=CARTESIAN_POINT('Ctrl Pts',(-13.2877292281856,-0.109420047168152,
2.05821110882994));
#30677=CARTESIAN_POINT('Ctrl Pts',(-13.3247424015232,0.514112789494058,
1.88846114794432));
#30678=CARTESIAN_POINT('Ctrl Pts',(-13.3617555748607,1.13764562615628,1.71871118705871));
#30679=CARTESIAN_POINT('Ctrl Pts',(-13.3987687481983,1.66880826384543,1.20966304967725));
#30680=CARTESIAN_POINT('Ctrl Pts',(-13.4357819215359,1.86490503196531,0.593907980555089));
#30681=CARTESIAN_POINT('Ctrl Pts',(-13.4727950948734,2.06100180008519,-0.02184708856707));
#30682=CARTESIAN_POINT('Ctrl Pts',(-13.509808268211,1.9220326986358,-0.744309089429943));
#30683=CARTESIAN_POINT('Ctrl Pts',(-13.5468214415486,1.51149466221922,-1.24337498515105));
#30684=CARTESIAN_POINT('Ctrl Pts',(-13.5838346148861,1.10095662580263,-1.74244088087216));
#30685=CARTESIAN_POINT('Ctrl Pts',(-13.6208477882237,0.418849654418843,
-2.01811067145151));
#30686=CARTESIAN_POINT('Ctrl Pts',(-13.6578609615612,-0.223161994900548,
-1.94442695713893));
#30687=CARTESIAN_POINT('Ctrl Pts',(-13.6948741348988,-0.86517364421993,
-1.87074324282635));
#30688=CARTESIAN_POINT('Ctrl Pts',(-13.7318873082364,-1.46708997147491,
-1.44770602362185));
#30689=CARTESIAN_POINT('Ctrl Pts',(-13.7689004815739,-1.7538869514037,-0.868606947538646));
#30690=CARTESIAN_POINT('Ctrl Pts',(-13.7859770903412,-1.88620524190027,
-0.601430494723484));
#30691=CARTESIAN_POINT('Ctrl Pts',(-13.8030536991085,-1.95144775983979,
-0.301034978383196));
#30692=CARTESIAN_POINT('Ctrl Pts',(-13.8201303078758,-1.95088537187799,
-0.000408160563786925));
#30693=CARTESIAN_POINT('Ctrl Pts',(-13.9218696921242,-1.95094021917743,
-0.000529095196661905));
#30694=CARTESIAN_POINT('Ctrl Pts',(-13.9052281145295,-1.95165179825443,
-0.29347677331393));
#30695=CARTESIAN_POINT('Ctrl Pts',(-13.8885865369347,-1.88983018220934,
-0.586139193047371));
#30696=CARTESIAN_POINT('Ctrl Pts',(-13.87194495934,-1.76394161972146,-0.848001901607685));
#30697=CARTESIAN_POINT('Ctrl Pts',(-13.8349317860024,-1.48394802187595,
-1.43042083198849));
#30698=CARTESIAN_POINT('Ctrl Pts',(-13.7979186126648,-0.887028563168493,
-1.86047999622125));
#30699=CARTESIAN_POINT('Ctrl Pts',(-13.7609054393273,-0.245924129428696,
-1.94167932096949));
#30700=CARTESIAN_POINT('Ctrl Pts',(-13.7238922659897,0.395180304311114,
-2.02287864571773));
#30701=CARTESIAN_POINT('Ctrl Pts',(-13.6868790926521,1.08046971308327,-1.75521813098144));
#30702=CARTESIAN_POINT('Ctrl Pts',(-13.6498659193146,1.49682573950857,-1.26099562586887));
#30703=CARTESIAN_POINT('Ctrl Pts',(-13.612852745977,1.91318176593387,-0.766773120756301));
#30704=CARTESIAN_POINT('Ctrl Pts',(-13.5758395726394,2.06060441001232,-0.04598862526747));
#30705=CARTESIAN_POINT('Ctrl Pts',(-13.5388263993019,1.87173419476462,0.57202129948511));
#30706=CARTESIAN_POINT('Ctrl Pts',(-13.5018132259643,1.68286397951692,1.1900312242377));
#30707=CARTESIAN_POINT('Ctrl Pts',(-13.4648000526268,1.15770090494307,1.70526657825403));
#30708=CARTESIAN_POINT('Ctrl Pts',(-13.4277868792892,0.536199356973832,
1.8823090905844));
#30709=CARTESIAN_POINT('Ctrl Pts',(-13.3907737059516,-0.085302190995406,
2.05935160291476));
#30710=CARTESIAN_POINT('Ctrl Pts',(-13.3537605326141,-0.803142212360044,
1.89820127355916));
#30711=CARTESIAN_POINT('Ctrl Pts',(-13.3167473592765,-1.28932951759698,
1.47248995173785));
#30712=CARTESIAN_POINT('Ctrl Pts',(-13.2851214702257,-1.70475203846754,
1.10874110727149));
#30713=CARTESIAN_POINT('Ctrl Pts',(-13.253495581175,-1.95104861266841,0.55184050939348));
#30714=CARTESIAN_POINT('Ctrl Pts',(-13.2218696921242,-1.95566871115984,
-0.00146207300122905));
#30715=CARTESIAN_POINT('Origin',(-9.8,0.,0.));
#30716=CARTESIAN_POINT('',(-12.4201303078758,-1.95564737559935,0.00146991064532538));
#30717=CARTESIAN_POINT('',(-12.5218696921242,-1.95543514278731,0.00154130734549634));
#30718=CARTESIAN_POINT('',(-9.8,-1.954,-2.39295984553393E-16));
#30719=CARTESIAN_POINT('Ctrl Pts',(-12.4201303078758,-1.95564737559935,
0.00146991064532538));
#30720=CARTESIAN_POINT('Ctrl Pts',(-12.4255622857244,-1.95644383279381,
0.0965063867288474));
#30721=CARTESIAN_POINT('Ctrl Pts',(-12.430994263573,-1.95011384225001,0.191436345000714));
#30722=CARTESIAN_POINT('Ctrl Pts',(-12.4364262414216,-1.93629099486106,
0.285262424508588));
#30723=CARTESIAN_POINT('Ctrl Pts',(-12.4734394147592,-1.84210293653611,
0.924587738637213));
#30724=CARTESIAN_POINT('Ctrl Pts',(-12.5104525880968,-1.40002315460498,
1.51266020037653));
#30725=CARTESIAN_POINT('Ctrl Pts',(-12.5474657614343,-0.812044111488547,
1.78078124108868));
#30726=CARTESIAN_POINT('Ctrl Pts',(-12.5844789347719,-0.2240650683721,2.04890228180084));
#30727=CARTESIAN_POINT('Ctrl Pts',(-12.6214921081094,0.50981323592966,1.99707190148582));
#30728=CARTESIAN_POINT('Ctrl Pts',(-12.658505281447,1.05427149512405,1.64897212898989));
#30729=CARTESIAN_POINT('Ctrl Pts',(-12.6955184547846,1.59872975431843,1.30087235649397));
#30730=CARTESIAN_POINT('Ctrl Pts',(-12.7325316281221,1.95376796840545,0.656503191817144));
#30731=CARTESIAN_POINT('Ctrl Pts',(-12.7695448014597,1.95716419001697,0.010285957989807));
#30732=CARTESIAN_POINT('Ctrl Pts',(-12.8065579747973,1.9605604116285,-0.635931275837539));
#30733=CARTESIAN_POINT('Ctrl Pts',(-12.8435711481348,1.61231464076452,-1.28399657881539));
#30734=CARTESIAN_POINT('Ctrl Pts',(-12.8805843214724,1.07154526206863,-1.63779981040261));
#30735=CARTESIAN_POINT('Ctrl Pts',(-12.91759749481,0.530775883372733,-1.99160304198983));
#30736=CARTESIAN_POINT('Ctrl Pts',(-12.9546106681475,-0.202517103155076,
-2.05114420218641));
#30737=CARTESIAN_POINT('Ctrl Pts',(-12.9916238414851,-0.793281831135205,
-1.78921809850206));
#30738=CARTESIAN_POINT('Ctrl Pts',(-13.0286370148227,-1.38404655911533,
-1.52729199481771));
#30739=CARTESIAN_POINT('Ctrl Pts',(-13.0656501881602,-1.83228302854778,
-0.943898627252431));
#30740=CARTESIAN_POINT('Ctrl Pts',(-13.1026633614978,-1.93318570000708,
-0.305598620587008));
#30741=CARTESIAN_POINT('Ctrl Pts',(-13.1084856769571,-1.94905808086367,
-0.205191558414774));
#30742=CARTESIAN_POINT('Ctrl Pts',(-13.1143079924164,-1.95633585779087,
-0.103425858474165));
#30743=CARTESIAN_POINT('Ctrl Pts',(-13.1201303078758,-1.95545730741116,
-0.00153438558903124));
#30744=CARTESIAN_POINT('Ctrl Pts',(-13.2218696921242,-1.95566871115984,
-0.00146207300122905));
#30745=CARTESIAN_POINT('Ctrl Pts',(-13.2164824078374,-1.95645571777858,
-0.0957139153194285));
#30746=CARTESIAN_POINT('Ctrl Pts',(-13.2110951235506,-1.95022996916634,
-0.189861353591568));
#30747=CARTESIAN_POINT('Ctrl Pts',(-13.2057078392638,-1.93663285562017,
-0.282931874217572));
#30748=CARTESIAN_POINT('Ctrl Pts',(-13.1686946659262,-1.84321429929716,
-0.922370064064672));
#30749=CARTESIAN_POINT('Ctrl Pts',(-13.1316814925887,-1.4018425975419,-1.51097412947185));
#30750=CARTESIAN_POINT('Ctrl Pts',(-13.0946683192511,-0.814186680996224,
-1.77980260461776));
#30751=CARTESIAN_POINT('Ctrl Pts',(-13.0576551459135,-0.226530764450553,
-2.04863107976367));
#30752=CARTESIAN_POINT('Ctrl Pts',(-13.020641972576,0.507409366885524,-1.99768396464832));
#30753=CARTESIAN_POINT('Ctrl Pts',(-12.9836287992384,1.05228615707883,-1.6502397118407));
#30754=CARTESIAN_POINT('Ctrl Pts',(-12.9466156259009,1.59716294727213,-1.30279545903307));
#30755=CARTESIAN_POINT('Ctrl Pts',(-12.9096024525633,1.95297639632267,-0.658854068533187));
#30756=CARTESIAN_POINT('Ctrl Pts',(-12.8725892792257,1.95715034111747,-0.0126414073408709));
#30757=CARTESIAN_POINT('Ctrl Pts',(-12.8355761058882,1.96132428591228,0.633571253851449));
#30758=CARTESIAN_POINT('Ctrl Pts',(-12.7985629325506,1.61385872645134,1.28205518573619));
#30759=CARTESIAN_POINT('Ctrl Pts',(-12.761549759213,1.07351555782829,1.63650897034401));
#30760=CARTESIAN_POINT('Ctrl Pts',(-12.7245365858755,0.533172389205236,
1.99096275495183));
#30761=CARTESIAN_POINT('Ctrl Pts',(-12.6875234125379,-0.20004838857994,
2.05138639228274));
#30762=CARTESIAN_POINT('Ctrl Pts',(-12.6505102392003,-0.791127902336491,
1.79017147364728));
#30763=CARTESIAN_POINT('Ctrl Pts',(-12.6134970658628,-1.38220741609303,
1.52895655501182));
#30764=CARTESIAN_POINT('Ctrl Pts',(-12.5764838925252,-1.83114566582096,
0.946103080410012));
#30765=CARTESIAN_POINT('Ctrl Pts',(-12.5394707191876,-1.93281645881963,
0.307924989943551));
#30766=CARTESIAN_POINT('Ctrl Pts',(-12.5336037101665,-1.94893243607642,
0.206766502944533));
#30767=CARTESIAN_POINT('Ctrl Pts',(-12.5277367011454,-1.95632302115412,
0.104217937603238));
#30768=CARTESIAN_POINT('Ctrl Pts',(-12.5218696921242,-1.95543514278731,
0.00154130734549634));
#30769=CARTESIAN_POINT('Origin',(-9.8,0.,0.));
#30770=CARTESIAN_POINT('',(-11.7201303078758,-1.95093397599971,0.000516778435547954));
#30771=CARTESIAN_POINT('',(-11.8218696921242,-1.95088048851305,0.000395614960693866));
#30772=CARTESIAN_POINT('',(-9.8,-1.954,-2.39295984553393E-16));
#30773=CARTESIAN_POINT('Ctrl Pts',(-11.7201303078758,-1.95093397599971,
0.000516778435547954));
#30774=CARTESIAN_POINT('Ctrl Pts',(-11.7368165790323,-1.9516307292599,0.294253588167556));
#30775=CARTESIAN_POINT('Ctrl Pts',(-11.7535028501889,-1.88946238212134,
0.587710338684493));
#30776=CARTESIAN_POINT('Ctrl Pts',(-11.7701891213455,-1.76291981471983,
0.850124222972598));
#30777=CARTESIAN_POINT('Ctrl Pts',(-11.807202294683,-1.48222546798021,1.43220577338039));
#30778=CARTESIAN_POINT('Ctrl Pts',(-11.8442154680206,-0.884788847197,1.86154624200128));
#30779=CARTESIAN_POINT('Ctrl Pts',(-11.8812286413582,-0.243587136816991,
1.94197393761962));
#30780=CARTESIAN_POINT('Ctrl Pts',(-11.9182418146957,0.397614573562981,
2.02240163323796));
#30781=CARTESIAN_POINT('Ctrl Pts',(-11.9552549880333,1.08258137353975,1.75391655585379));
#30782=CARTESIAN_POINT('Ctrl Pts',(-11.9922681613709,1.49834231022453,1.25919330883212));
#30783=CARTESIAN_POINT('Ctrl Pts',(-12.0292813347084,1.91410324690933,0.764470061810429));
#30784=CARTESIAN_POINT('Ctrl Pts',(-12.066294508046,2.06065832030212,0.0435086451512185));
#30785=CARTESIAN_POINT('Ctrl Pts',(-12.1033076813835,1.87104445865698,-0.574273542264962));
#30786=CARTESIAN_POINT('Ctrl Pts',(-12.1403208547211,1.68143059701185,-1.19205572968113));
#30787=CARTESIAN_POINT('Ctrl Pts',(-12.1773340280587,1.15564780032879,-1.70665868785428));
#30788=CARTESIAN_POINT('Ctrl Pts',(-12.2143472013962,0.533933614275722,
-1.88295309637894));
#30789=CARTESIAN_POINT('Ctrl Pts',(-12.2513603747338,-0.0877805717773474,
-2.0592475049036));
#30790=CARTESIAN_POINT('Ctrl Pts',(-12.2883735480714,-0.805426147200425,
-1.89723336377978));
#30791=CARTESIAN_POINT('Ctrl Pts',(-12.3253867214089,-1.29110076755259,
-1.4709372099589));
#30792=CARTESIAN_POINT('Ctrl Pts',(-12.3569679168979,-1.70549877091952,
-1.10720341044869));
#30793=CARTESIAN_POINT('Ctrl Pts',(-12.3885491123868,-1.95101682093624,
-0.551066497531743));
#30794=CARTESIAN_POINT('Ctrl Pts',(-12.4201303078758,-1.95564737559935,
0.00146991064532538));
#30795=CARTESIAN_POINT('Ctrl Pts',(-12.5218696921242,-1.95543514278731,
0.00154130734549634));
#30796=CARTESIAN_POINT('Ctrl Pts',(-12.4907235278078,-1.95072166690785,
-0.543537656389124));
#30797=CARTESIAN_POINT('Ctrl Pts',(-12.4595773634914,-1.71270248299415,
-1.09222577733106));
#30798=CARTESIAN_POINT('Ctrl Pts',(-12.428431199175,-1.30824303327262,-1.45571200064073));
#30799=CARTESIAN_POINT('Ctrl Pts',(-12.3914180258374,-0.827595478457534,
-1.88766819442741));
#30800=CARTESIAN_POINT('Ctrl Pts',(-12.3544048524998,-0.111897032557945,
-2.05807787566966));
#30801=CARTESIAN_POINT('Ctrl Pts',(-12.3173916791623,0.511839630816549,
-1.88907846720071));
#30802=CARTESIAN_POINT('Ctrl Pts',(-12.2803785058247,1.13557629419105,-1.72007905873176));
#30803=CARTESIAN_POINT('Ctrl Pts',(-12.2433653324871,1.66735117504045,-1.21167056055161));
#30804=CARTESIAN_POINT('Ctrl Pts',(-12.2063521591496,1.86418886026822,-0.596151957279062));
#30805=CARTESIAN_POINT('Ctrl Pts',(-12.169338985812,2.061026545496,0.0193666459934833));
#30806=CARTESIAN_POINT('Ctrl Pts',(-12.1323258124744,1.92292703510214,0.741995354358439));
#30807=CARTESIAN_POINT('Ctrl Pts',(-12.0953126391369,1.51298993531999,1.2415549599338));
#30808=CARTESIAN_POINT('Ctrl Pts',(-12.0582994657993,1.10305283553785,1.74111456550915));
#30809=CARTESIAN_POINT('Ctrl Pts',(-12.0212862924617,0.421278146367432,
2.01760506829494));
#30810=CARTESIAN_POINT('Ctrl Pts',(-11.9842731191242,-0.220821699570658,
1.94469407360503));
#30811=CARTESIAN_POINT('Ctrl Pts',(-11.9472599457866,-0.862921545508766,
1.87178307891512));
#30812=CARTESIAN_POINT('Ctrl Pts',(-11.9102467724491,-1.46534654821454,
1.4494705867495));
#30813=CARTESIAN_POINT('Ctrl Pts',(-11.8732335991115,-1.75284026146716,
0.870717107156824));
#30814=CARTESIAN_POINT('Ctrl Pts',(-11.8561122967824,-1.8858271506868,0.603001253459379));
#30815=CARTESIAN_POINT('Ctrl Pts',(-11.8389909944533,-1.95142694075535,
0.30181110017949));
#30816=CARTESIAN_POINT('Ctrl Pts',(-11.8218696921242,-1.95088048851305,
0.000395614960693866));
#30817=CARTESIAN_POINT('Origin',(-9.8,0.,0.));
#30818=CARTESIAN_POINT('',(-11.0201303078758,-1.95375977033508,-0.00177812828496077));
#30819=CARTESIAN_POINT('',(-11.1218696921242,-1.95398910254737,-0.00177651513874471));
#30820=CARTESIAN_POINT('',(-9.8,-1.954,-2.39295984553393E-16));
#30821=CARTESIAN_POINT('Ctrl Pts',(-11.0201303078758,-1.95375977033508,
-0.00177812828496077));
#30822=CARTESIAN_POINT('Ctrl Pts',(-11.0480708723403,-1.94931821586781,
0.488280492828455));
#30823=CARTESIAN_POINT('Ctrl Pts',(-11.0760114368048,-1.762242579831,0.981361839095669));
#30824=CARTESIAN_POINT('Ctrl Pts',(-11.1039520012693,-1.42887346982972,
1.33750442049114));
#30825=CARTESIAN_POINT('Ctrl Pts',(-11.1409651746069,-0.987255739825101,
1.8092904187597));
#30826=CARTESIAN_POINT('Ctrl Pts',(-11.1779783479444,-0.288913552828485,
2.04076815788204));
#30827=CARTESIAN_POINT('Ctrl Pts',(-11.214991521282,0.347070736053018,1.92617220720064));
#30828=CARTESIAN_POINT('Ctrl Pts',(-11.2520046946196,0.983055024934531,
1.81157625651923));
#30829=CARTESIAN_POINT('Ctrl Pts',(-11.2890178679571,1.55668141570094,1.35090661603405));
#30830=CARTESIAN_POINT('Ctrl Pts',(-11.3260310412947,1.80585195247114,0.754649715677886));
#30831=CARTESIAN_POINT('Ctrl Pts',(-11.3630442146323,2.05502248924135,0.158392815321727));
#30832=CARTESIAN_POINT('Ctrl Pts',(-11.4000573879698,1.97973717201537,-0.573451344905431));
#30833=CARTESIAN_POINT('Ctrl Pts',(-11.4370705613074,1.61439491979416,-1.10649288771296));
#30834=CARTESIAN_POINT('Ctrl Pts',(-11.474083734645,1.24905266757295,-1.6395344305205));
#30835=CARTESIAN_POINT('Ctrl Pts',(-11.5110969079825,0.59365348035652,-1.97377335590839));
#30836=CARTESIAN_POINT('Ctrl Pts',(-11.5481100813201,-0.0523415465836445,
-1.95649120369037));
#30837=CARTESIAN_POINT('Ctrl Pts',(-11.5851232546576,-0.698336573523782,
-1.93920905147235));
#30838=CARTESIAN_POINT('Ctrl Pts',(-11.6221364279952,-1.33492744018764,
-1.57040582164844));
#30839=CARTESIAN_POINT('Ctrl Pts',(-11.6591496013328,-1.67124683717155,
-1.01859289063916));
#30840=CARTESIAN_POINT('Ctrl Pts',(-11.6794765035138,-1.85594679309579,
-0.71554815117469));
#30841=CARTESIAN_POINT('Ctrl Pts',(-11.6998034056948,-1.95008520426206,
-0.357307887264606));
#30842=CARTESIAN_POINT('Ctrl Pts',(-11.7201303078758,-1.95093397599971,
0.000516778435547954));
#30843=CARTESIAN_POINT('Ctrl Pts',(-11.8218696921242,-1.95088048851305,
0.000395614960693866));
#30844=CARTESIAN_POINT('Ctrl Pts',(-11.8019778211157,-1.95024560938371,
-0.34979491591636));
#30845=CARTESIAN_POINT('Ctrl Pts',(-11.7820859501073,-1.86032483576546,
-0.700289605624201));
#30846=CARTESIAN_POINT('Ctrl Pts',(-11.7621940790988,-1.68306414685726,
-0.998945614375208));
#30847=CARTESIAN_POINT('Ctrl Pts',(-11.7251809057612,-1.35323189519527,
-1.55466038929485));
#30848=CARTESIAN_POINT('Ctrl Pts',(-11.6881677324237,-0.721004968071823,
-1.93089547211442));
#30849=CARTESIAN_POINT('Ctrl Pts',(-11.6511545590861,-0.0752567296127299,
-1.95574376838169));
#30850=CARTESIAN_POINT('Ctrl Pts',(-11.6141413857485,0.570491508846364,
-1.98059206464896));
#30851=CARTESIAN_POINT('Ctrl Pts',(-11.577128212411,1.22976105864111,-1.65405357436393));
#30852=CARTESIAN_POINT('Ctrl Pts',(-11.5401150390734,1.60132240146957,-1.12532832074356));
#30853=CARTESIAN_POINT('Ctrl Pts',(-11.5031018657358,1.97288374429803,-0.596603067123194));
#30854=CARTESIAN_POINT('Ctrl Pts',(-11.4660886923983,2.0567368801602,0.134308949832498));
#30855=CARTESIAN_POINT('Ctrl Pts',(-11.4290755190607,1.81456813336496,0.733443762187807));
#30856=CARTESIAN_POINT('Ctrl Pts',(-11.3920623457231,1.57239938656973,1.33257857454311));
#30857=CARTESIAN_POINT('Ctrl Pts',(-11.3550491723856,1.00420875711708,1.79993618229802));
#30858=CARTESIAN_POINT('Ctrl Pts',(-11.318035999048,0.369610525185732,1.9219743293259));
#30859=CARTESIAN_POINT('Ctrl Pts',(-11.2810228257105,-0.264987706745639,
2.04401247635378));
#30860=CARTESIAN_POINT('Ctrl Pts',(-11.2440096523729,-0.965993541155731,
1.82073116265462));
#30861=CARTESIAN_POINT('Ctrl Pts',(-11.2069964790353,-1.41310756501697,
1.35415075697192));
#30862=CARTESIAN_POINT('Ctrl Pts',(-11.1786208833983,-1.75588084276393,
0.996453868810782));
#30863=CARTESIAN_POINT('Ctrl Pts',(-11.1502452877613,-1.94943446818612,
0.495762979235285));
#30864=CARTESIAN_POINT('Ctrl Pts',(-11.1218696921242,-1.95398910254737,
-0.00177651513874471));
#30865=CARTESIAN_POINT('Origin',(-9.8,0.,0.));
#30866=CARTESIAN_POINT('',(-10.3201303078758,-1.9568945579723,0.000687273504990336));
#30867=CARTESIAN_POINT('',(-10.4218696921242,-1.95677370715668,0.000813444693687295));
#30868=CARTESIAN_POINT('',(-9.8,-1.954,-2.39295984553393E-16));
#30869=CARTESIAN_POINT('Ctrl Pts',(-10.3201303078758,-1.9568945579723,0.000687273504990337));
#30870=CARTESIAN_POINT('Ctrl Pts',(-10.3223119923107,-1.95706803944366,
0.0387935361464464));
#30871=CARTESIAN_POINT('Ctrl Pts',(-10.3244936767456,-1.95605118783441,
0.0768903607640225));
#30872=CARTESIAN_POINT('Ctrl Pts',(-10.3266753611805,-1.95381470630591,
0.114915451699472));
#30873=CARTESIAN_POINT('Ctrl Pts',(-10.363688534518,-1.91587187774813,0.760026751691749));
#30874=CARTESIAN_POINT('Ctrl Pts',(-10.4007017078556,-1.52688885554805,
1.38449129214901));
#30875=CARTESIAN_POINT('Ctrl Pts',(-10.4377148811932,-0.964597446735795,
1.70298245245432));
#30876=CARTESIAN_POINT('Ctrl Pts',(-10.4747280545307,-0.402306037923545,
2.02147361275964));
#30877=CARTESIAN_POINT('Ctrl Pts',(-10.5117412278683,0.333293757500867,
2.03399139291301));
#30878=CARTESIAN_POINT('Ctrl Pts',(-10.5487544012059,0.906096059768414,
1.73481624332052));
#30879=CARTESIAN_POINT('Ctrl Pts',(-10.5857675745434,1.47889836203597,1.43564109372802));
#30880=CARTESIAN_POINT('Ctrl Pts',(-10.622780747881,1.88890317114665,0.824773014389662));
#30881=CARTESIAN_POINT('Ctrl Pts',(-10.6597939212185,1.94877353033013,0.181326211842671));
#30882=CARTESIAN_POINT('Ctrl Pts',(-10.6968070945561,2.00864388951361,-0.462120590704301));
#30883=CARTESIAN_POINT('Ctrl Pts',(-10.7338202678937,1.71837979876989,-1.13814611645991));
#30884=CARTESIAN_POINT('Ctrl Pts',(-10.7708334412312,1.21060699860575,-1.53786480632835));
#30885=CARTESIAN_POINT('Ctrl Pts',(-10.8078466145688,0.702834198441578,
-1.93758349619681));
#30886=CARTESIAN_POINT('Ctrl Pts',(-10.8448597879064,-0.0224473111430409,
-2.06099535017809));
#30887=CARTESIAN_POINT('Ctrl Pts',(-10.8818729612439,-0.63384622012401,
-1.85171175857666));
#30888=CARTESIAN_POINT('Ctrl Pts',(-10.9188861345815,-1.24524512910496,
-1.64242816697523));
#30889=CARTESIAN_POINT('Ctrl Pts',(-10.9558993079191,-1.74276143748226,
-1.10044912979111));
#30890=CARTESIAN_POINT('Ctrl Pts',(-10.9929124812566,-1.89907295516461,
-0.473412482491661));
#30891=CARTESIAN_POINT('Ctrl Pts',(-11.0019850901297,-1.93738778025002,
-0.319714278932262));
#30892=CARTESIAN_POINT('Ctrl Pts',(-11.0110576990027,-1.95520199196668,
-0.160905557506181));
#30893=CARTESIAN_POINT('Ctrl Pts',(-11.0201303078758,-1.95375977033508,
-0.00177812828496077));
#30894=CARTESIAN_POINT('Ctrl Pts',(-11.1218696921242,-1.95398910254737,
-0.00177651513874471));
#30895=CARTESIAN_POINT('Ctrl Pts',(-11.1132321144237,-1.95537554069288,
-0.153228350607148));
#30896=CARTESIAN_POINT('Ctrl Pts',(-11.1045945367232,-1.93924926518043,
-0.304388176676578));
#30897=CARTESIAN_POINT('Ctrl Pts',(-11.0959569590226,-1.90448826142854,
-0.45113382160585));
#30898=CARTESIAN_POINT('Ctrl Pts',(-11.0589437856851,-1.75553272066649,
-1.07995849683472));
#30899=CARTESIAN_POINT('Ctrl Pts',(-11.0219306123475,-1.26439942583,-1.62772834962624));
#30900=CARTESIAN_POINT('Ctrl Pts',(-10.9849174390099,-0.655494078459054,
-1.84415963951631));
#30901=CARTESIAN_POINT('Ctrl Pts',(-10.9479042656724,-0.0465887310881076,
-2.06059092940637));
#30902=CARTESIAN_POINT('Ctrl Pts',(-10.9108910923348,0.680088668817298,
-1.94568365639498));
#30903=CARTESIAN_POINT('Ctrl Pts',(-10.8738779189972,1.19250900933691,-1.55194056766556));
#30904=CARTESIAN_POINT('Ctrl Pts',(-10.8368647456597,1.70492934985651,-1.15819747893615));
#30905=CARTESIAN_POINT('Ctrl Pts',(-10.7998515723221,2.00309263099032,-0.485618574488742));
#30906=CARTESIAN_POINT('Ctrl Pts',(-10.7628383989846,1.95076386117954,0.158485396272577));
#30907=CARTESIAN_POINT('Ctrl Pts',(-10.725825225647,1.89843509136877,0.802589367033887));
#30908=CARTESIAN_POINT('Ctrl Pts',(-10.6888120523094,1.4956142706134,1.4182184041091));
#30909=CARTESIAN_POINT('Ctrl Pts',(-10.6517988789719,0.926355890488103,
1.72408295249208));
#30910=CARTESIAN_POINT('Ctrl Pts',(-10.6147857056343,0.357097510362794,
2.02994750087506));
#30911=CARTESIAN_POINT('Ctrl Pts',(-10.5777725322967,-0.378598429132457,
2.02604756056581));
#30912=CARTESIAN_POINT('Ctrl Pts',(-10.5407593589592,-0.944582118652054,
1.7141650690755));
#30913=CARTESIAN_POINT('Ctrl Pts',(-10.5037461856216,-1.51056580817164,
1.40228257758519));
#30914=CARTESIAN_POINT('Ctrl Pts',(-10.466733012284,-1.90683724771558,0.782417534913847));
#30915=CARTESIAN_POINT('Ctrl Pts',(-10.4297198389465,-1.95233444998628,
0.137794986529184));
#30916=CARTESIAN_POINT('Ctrl Pts',(-10.4271031233391,-1.95555095990802,
0.092222188221208));
#30917=CARTESIAN_POINT('Ctrl Pts',(-10.4244864077316,-1.95701428341649,
0.0465256507156762));
#30918=CARTESIAN_POINT('Ctrl Pts',(-10.4218696921242,-1.95677370715668,
0.000813444693687295));
#30919=CARTESIAN_POINT('Origin',(-9.8,0.,0.));
#30920=CARTESIAN_POINT('',(-9.62013030787576,-1.951759122336,0.00130501714239645));
#30921=CARTESIAN_POINT('',(-9.72186969212421,-1.95160825484864,0.00121583516621696));
#30922=CARTESIAN_POINT('',(-9.8,-1.954,-2.39295984553393E-16));
#30923=CARTESIAN_POINT('Ctrl Pts',(-9.62013030787576,-1.951759122336,0.00130501714239645));
#30924=CARTESIAN_POINT('Ctrl Pts',(-9.63356628561861,-1.95321216672716,
0.23757493874278));
#30925=CARTESIAN_POINT('Ctrl Pts',(-9.64700226336145,-1.91351631519969,
0.473373218815082));
#30926=CARTESIAN_POINT('Ctrl Pts',(-9.6604382411043,-1.8304828450213,0.692769818698314));
#30927=CARTESIAN_POINT('Ctrl Pts',(-9.69745141444186,-1.60174383671438,
1.29715935674101));
#30928=CARTESIAN_POINT('Ctrl Pts',(-9.73446458777943,-1.04412356331037,
1.77707954233155));
#30929=CARTESIAN_POINT('Ctrl Pts',(-9.77147776111699,-0.412406560823673,
1.91324810105907));
#30930=CARTESIAN_POINT('Ctrl Pts',(-9.80849093445456,0.21931044166301,2.04941665978659));
#30931=CARTESIAN_POINT('Ctrl Pts',(-9.84550410779212,0.925124173232371,
1.8418335916511));
#30932=CARTESIAN_POINT('Ctrl Pts',(-9.88251728112969,1.38253842510649,1.38534651647905));
#30933=CARTESIAN_POINT('Ctrl Pts',(-9.91953045446725,1.83995267698061,0.928859441306994));
#30934=CARTESIAN_POINT('Ctrl Pts',(-9.95654362780481,2.04896744915949,0.223468359098379));
#30935=CARTESIAN_POINT('Ctrl Pts',(-9.99355680114238,1.91408095612756,-0.408523635798906));
#30936=CARTESIAN_POINT('Ctrl Pts',(-10.0305699744799,1.77919446309564,-1.04051563069619));
#30937=CARTESIAN_POINT('Ctrl Pts',(-10.0675831478175,1.30040670485291,-1.59910853828215));
#30938=CARTESIAN_POINT('Ctrl Pts',(-10.1045963211551,0.696482533847406,
-1.82907341232167));
#30939=CARTESIAN_POINT('Ctrl Pts',(-10.1416094944926,0.0925583628419107,
-2.0590382863612));
#30940=CARTESIAN_POINT('Ctrl Pts',(-10.1786226678302,-0.636502220926357,
-1.96037512685431));
#30941=CARTESIAN_POINT('Ctrl Pts',(-10.2156358411678,-1.15758119535276,
-1.57816451733723));
#30942=CARTESIAN_POINT('Ctrl Pts',(-10.2504673300704,-1.64794597303924,
-1.21848272289988));
#30943=CARTESIAN_POINT('Ctrl Pts',(-10.2852988189731,-1.95412485496321,
-0.607694875208273));
#30944=CARTESIAN_POINT('Ctrl Pts',(-10.3201303078758,-1.9568945579723,0.000687273504990337));
#30945=CARTESIAN_POINT('Ctrl Pts',(-10.4218696921242,-1.95677370715668,
0.000813444693687295));
#30946=CARTESIAN_POINT('Ctrl Pts',(-10.3874732343941,-1.95361135694641,
-0.600068805456268));
#30947=CARTESIAN_POINT('Ctrl Pts',(-10.3530767766639,-1.65603502305887,
-1.20365839229021));
#30948=CARTESIAN_POINT('Ctrl Pts',(-10.3186803189338,-1.17598871060954,
-1.56449602602075));
#30949=CARTESIAN_POINT('Ctrl Pts',(-10.2816671455962,-0.659422803964663,
-1.95278443608801));
#30950=CARTESIAN_POINT('Ctrl Pts',(-10.2446539722586,0.0684319743225153,
-2.05998120212456));
#30951=CARTESIAN_POINT('Ctrl Pts',(-10.2076407989211,0.675008551610066,
-1.83710661589606));
#30952=CARTESIAN_POINT('Ctrl Pts',(-10.1706276255835,1.28158512889762,-1.61423202966757));
#30953=CARTESIAN_POINT('Ctrl Pts',(-10.133614452246,1.76688350518553,-1.06128609117405));
#30954=CARTESIAN_POINT('Ctrl Pts',(-10.0966012789084,1.90916403518392,-0.430917567147205));
#30955=CARTESIAN_POINT('Ctrl Pts',(-10.0595881055708,2.05144456518231,0.199450956879657));
#30956=CARTESIAN_POINT('Ctrl Pts',(-10.0225749322333,1.85070724889113,0.907242066439859));
#30957=CARTESIAN_POINT('Ctrl Pts',(-9.9855617588957,1.39867178595441,1.36905606097446));
#30958=CARTESIAN_POINT('Ctrl Pts',(-9.94854858555813,0.946636323017702,
1.83087005550905));
#30959=CARTESIAN_POINT('Ctrl Pts',(-9.91153541222057,0.243302713435483,
2.04670693501808));
#30960=CARTESIAN_POINT('Ctrl Pts',(-9.87452223888301,-0.389966036589458,
1.91794779731423));
#30961=CARTESIAN_POINT('Ctrl Pts',(-9.83750906554544,-1.02323478661442,
1.78918865961037));
#30962=CARTESIAN_POINT('Ctrl Pts',(-9.80049589220787,-1.58643867708208,
1.31583350469361));
#30963=CARTESIAN_POINT('Ctrl Pts',(-9.76348271887031,-1.82224193890655,
0.71416495223856));
#30964=CARTESIAN_POINT('Ctrl Pts',(-9.74961170995494,-1.91061126399005,
0.488684424560365));
#30965=CARTESIAN_POINT('Ctrl Pts',(-9.73574070103958,-1.95299910665996,
0.245183038899142));
#30966=CARTESIAN_POINT('Ctrl Pts',(-9.72186969212421,-1.95160825484864,
0.00121583516621696));
#30967=CARTESIAN_POINT('Origin',(-9.8,0.,0.));
#30968=CARTESIAN_POINT('',(-8.92013030787576,-1.95219365985136,-0.00150278625351857));
#30969=CARTESIAN_POINT('',(-9.02186969212422,-1.95238063947443,-0.00156704507775435));
#30970=CARTESIAN_POINT('',(-9.8,-1.954,-2.39295984553393E-16));
#30971=CARTESIAN_POINT('Ctrl Pts',(-8.92013030787576,-1.95219365985136,
-0.00150278625351857));
#30972=CARTESIAN_POINT('Ctrl Pts',(-8.94482057892656,-1.94907401794518,
0.432429328865723));
#30973=CARTESIAN_POINT('Ctrl Pts',(-8.96951084997735,-1.80626939344938,
0.868225234004993));
#30974=CARTESIAN_POINT('Ctrl Pts',(-8.99420112102815,-1.54031802273755,
1.20748410194356));
#30975=CARTESIAN_POINT('Ctrl Pts',(-9.03121429436571,-1.1416304521042,1.71606690605629));
#30976=CARTESIAN_POINT('Ctrl Pts',(-9.06822746770327,-0.466195278319233,
2.00770208888324));
#30977=CARTESIAN_POINT('Ctrl Pts',(-9.10524064104083,0.177371679629828,
1.94913743868457));
#30978=CARTESIAN_POINT('Ctrl Pts',(-9.1422538143784,0.82093863757888,1.89057278848591));
#30979=CARTESIAN_POINT('Ctrl Pts',(-9.17926698771596,1.43263737969203,1.48180830526165));
#30980=CARTESIAN_POINT('Ctrl Pts',(-9.21628016105352,1.73297415794162,0.909614223461296));
#30981=CARTESIAN_POINT('Ctrl Pts',(-9.25329333439109,2.0333109361912,0.337420141660943));
#30982=CARTESIAN_POINT('Ctrl Pts',(-9.29030650772865,2.02228575057723,-0.398203538715502));
#30983=CARTESIAN_POINT('Ctrl Pts',(-9.32731968106622,1.70493616328153,-0.961140024528901));
#30984=CARTESIAN_POINT('Ctrl Pts',(-9.36433285440378,1.38758657598583,-1.52407651034231));
#30985=CARTESIAN_POINT('Ctrl Pts',(-9.40134602774135,0.763912587008396,
-1.91432580159266));
#30986=CARTESIAN_POINT('Ctrl Pts',(-9.43835920107891,0.118879602889872,
-1.95357751513302));
#30987=CARTESIAN_POINT('Ctrl Pts',(-9.47537237441648,-0.526153381228652,
-1.99282922867337));
#30988=CARTESIAN_POINT('Ctrl Pts',(-9.51238554775404,-1.19254536048827,
-1.68108336450373));
#30989=CARTESIAN_POINT('Ctrl Pts',(-9.54939872109161,-1.57581247851316,
-1.16078098717147));
#30990=CARTESIAN_POINT('Ctrl Pts',(-9.57297591668632,-1.81995160498805,
-0.829351125514365));
#30991=CARTESIAN_POINT('Ctrl Pts',(-9.59655311228104,-1.94920934795607,
-0.41329690177544));
#30992=CARTESIAN_POINT('Ctrl Pts',(-9.62013030787576,-1.951759122336,0.00130501714239645));
#30993=CARTESIAN_POINT('Ctrl Pts',(-9.72186969212421,-1.95160825484864,
0.00121583516621696));
#30994=CARTESIAN_POINT('Ctrl Pts',(-9.69872752770202,-1.94928778043318,
-0.405815057601631));
#30995=CARTESIAN_POINT('Ctrl Pts',(-9.67558536327982,-1.82510913530187,
-0.814142556830142));
#30996=CARTESIAN_POINT('Ctrl Pts',(-9.65244319885762,-1.58930196205156,
-1.14224189046578));
#30997=CARTESIAN_POINT('Ctrl Pts',(-9.61543002552006,-1.21215609019086,
-1.66699823072174));
#30998=CARTESIAN_POINT('Ctrl Pts',(-9.57841685218249,-0.549461713288179,
-1.98652896124034));
#30999=CARTESIAN_POINT('Ctrl Pts',(-9.54140367884493,0.0959867987391138,
-1.95483600268248));
#31000=CARTESIAN_POINT('Ctrl Pts',(-9.50439050550736,0.741435310766425,
-1.92314304412462));
#31001=CARTESIAN_POINT('Ctrl Pts',(-9.4673773321698,1.36963795791836,-1.54022639649028));
#31002=CARTESIAN_POINT('Ctrl Pts',(-9.43036415883223,1.69356012611861,-0.981046055053941));
#31003=CARTESIAN_POINT('Ctrl Pts',(-9.39335098549467,2.01748229431886,-0.421865713617614));
#31004=CARTESIAN_POINT('Ctrl Pts',(-9.3563378121571,2.03712398356746,0.313578321620689));
#31005=CARTESIAN_POINT('Ctrl Pts',(-9.31932463881954,1.74351063013272,0.889251339909027));
#31006=CARTESIAN_POINT('Ctrl Pts',(-9.28231146548198,1.44989727669798,1.46492435819737));
#31007=CARTESIAN_POINT('Ctrl Pts',(-9.24529829214442,0.843028880579888,
1.88082635953573));
#31008=CARTESIAN_POINT('Ctrl Pts',(-9.20828511880685,0.20019213686734,1.94692587718493));
#31009=CARTESIAN_POINT('Ctrl Pts',(-9.17127194546928,-0.442644606845208,
2.01302539483412));
#31010=CARTESIAN_POINT('Ctrl Pts',(-9.13425877213171,-1.12144969815222,
1.72932242879415));
#31011=CARTESIAN_POINT('Ctrl Pts',(-9.09724559879415,-1.52606755541189,
1.22544484952811));
#31012=CARTESIAN_POINT('Ctrl Pts',(-9.07212029657084,-1.80073046679972,
0.883402400285829));
#31013=CARTESIAN_POINT('Ctrl Pts',(-9.04699499434753,-1.94904863493835,
0.439904078837482));
#31014=CARTESIAN_POINT('Ctrl Pts',(-9.02186969212422,-1.95238063947443,
-0.00156704507775435));
#31015=CARTESIAN_POINT('Origin',(-9.8,0.,0.));
#31016=CARTESIAN_POINT('',(-8.22013030787576,-1.95711605195191,-0.000344670306376693));
#31017=CARTESIAN_POINT('',(-8.32186969212422,-1.95716419186761,-0.000205378326722651));
#31018=CARTESIAN_POINT('',(-9.8,-1.954,-2.39295984553393E-16));
#31019=CARTESIAN_POINT('Ctrl Pts',(-8.22013030787576,-1.95711605195191,
-0.000344670306376693));
#31020=CARTESIAN_POINT('Ctrl Pts',(-8.2560748722345,-1.95558481932104,0.627289137352789));
#31021=CARTESIAN_POINT('Ctrl Pts',(-8.29201943659324,-1.62669741337902,
1.25630241576526));
#31022=CARTESIAN_POINT('Ctrl Pts',(-8.32796400095198,-1.1097662979966,1.61214646711999));
#31023=CARTESIAN_POINT('Ctrl Pts',(-8.36497717428955,-0.577467150167943,
1.9785695352224));
#31024=CARTESIAN_POINT('Ctrl Pts',(-8.40199034762711,0.154222745866834,
2.05533964587135));
#31025=CARTESIAN_POINT('Ctrl Pts',(-8.43900352096467,0.750983998293585,
1.80737945709348));
#31026=CARTESIAN_POINT('Ctrl Pts',(-8.47601669430224,1.34774525072034,1.55941926831562));
#31027=CARTESIAN_POINT('Ctrl Pts',(-8.51302986763981,1.80957785953908,0.986728780110945));
#31028=CARTESIAN_POINT('Ctrl Pts',(-8.55004304097737,1.92546401824878,0.350978321333127));
#31029=CARTESIAN_POINT('Ctrl Pts',(-8.58705621431494,2.04135017695848,-0.284772137444683));
#31030=CARTESIAN_POINT('Ctrl Pts',(-8.62406938765249,1.81128988555918,-0.983582566795618));
#31031=CARTESIAN_POINT('Ctrl Pts',(-8.66108256099005,1.34040092293233,-1.42615666510335));
#31032=CARTESIAN_POINT('Ctrl Pts',(-8.69809573432762,0.869511960305483,
-1.86873076341109));
#31033=CARTESIAN_POINT('Ctrl Pts',(-8.73510890766519,0.157794326451077,
-2.05506853067559));
#31034=CARTESIAN_POINT('Ctrl Pts',(-8.77212208100276,-0.469558193964634,
-1.90002962347886));
#31035=CARTESIAN_POINT('Ctrl Pts',(-8.80913525434033,-1.09691071438035,
-1.74499071628214));
#31036=CARTESIAN_POINT('Ctrl Pts',(-8.84614842767788,-1.63989812135737,
-1.24857513462419));
#31037=CARTESIAN_POINT('Ctrl Pts',(-8.88316160101544,-1.85042184110501,
-0.637602131095955));
#31038=CARTESIAN_POINT('Ctrl Pts',(-8.89548450330222,-1.92051210880072,
-0.434189131252125));
#31039=CARTESIAN_POINT('Ctrl Pts',(-8.90780740558899,-1.95375067161119,
-0.218078094102745));
#31040=CARTESIAN_POINT('Ctrl Pts',(-8.92013030787576,-1.95219365985136,
-0.00150278625351857));
#31041=CARTESIAN_POINT('Ctrl Pts',(-9.02186969212422,-1.95238063947443,
-0.00156704507775435));
#31042=CARTESIAN_POINT('Ctrl Pts',(-9.00998182100997,-1.95395715545522,
-0.210446197062624));
#31043=CARTESIAN_POINT('Ctrl Pts',(-8.99809394989571,-1.92307638969601,
-0.418871531111766));
#31044=CARTESIAN_POINT('Ctrl Pts',(-8.98620607878146,-1.85776384109645,
-0.615882110172357));
#31045=CARTESIAN_POINT('Ctrl Pts',(-8.9491929054439,-1.65441164630902,-1.22927929811467));
#31046=CARTESIAN_POINT('Ctrl Pts',(-8.91217973210633,-1.11727663352183,
-1.73202148150718));
#31047=CARTESIAN_POINT('Ctrl Pts',(-8.87516655876876,-0.491783335409503,
-1.89439869455437));
#31048=CARTESIAN_POINT('Ctrl Pts',(-8.8381533854312,0.133709962702829,-2.05677590760156));
#31049=CARTESIAN_POINT('Ctrl Pts',(-8.80114021209364,0.84756154614031,-1.8787881503034));
#31050=CARTESIAN_POINT('Ctrl Pts',(-8.76412703875608,1.32360259869579,-1.44176052922861));
#31051=CARTESIAN_POINT('Ctrl Pts',(-8.72711386541851,1.79964365125125,-1.00473290815384));
#31052=CARTESIAN_POINT('Ctrl Pts',(-8.69010069208094,2.03787417292474,-0.308665423302459));
#31053=CARTESIAN_POINT('Ctrl Pts',(-8.65308751874338,1.9294432918523,0.328398913582165));
#31054=CARTESIAN_POINT('Ctrl Pts',(-8.61607434540581,1.82101241077986,0.965463250466808));
#31055=CARTESIAN_POINT('Ctrl Pts',(-8.57906117206825,1.36592012696147,1.54352443938468));
#31056=CARTESIAN_POINT('Ctrl Pts',(-8.54204799873069,0.772104497721655,
1.79845820288207));
#31057=CARTESIAN_POINT('Ctrl Pts',(-8.50503482539313,0.178288868481854,
2.05339196637945));
#31058=CARTESIAN_POINT('Ctrl Pts',(-8.46802165205556,-0.554250106179376,
1.98519830445635));
#31059=CARTESIAN_POINT('Ctrl Pts',(-8.431008478718,-1.09080507849613,1.62503585918676));
#31060=CARTESIAN_POINT('Ctrl Pts',(-8.39462888318673,-1.61817550132231,
1.27103854139505));
#31061=CARTESIAN_POINT('Ctrl Pts',(-8.35824928765548,-1.95621405916918,
0.634982516742313));
#31062=CARTESIAN_POINT('Ctrl Pts',(-8.32186969212422,-1.95716419186761,
-0.000205378326722651));
#31063=CARTESIAN_POINT('Origin',(-9.8,0.,0.));
#31064=CARTESIAN_POINT('',(-7.52013030787576,-1.95318687626922,0.00173935763946309));
#31065=CARTESIAN_POINT('',(-7.62186969212422,-1.95297113082797,0.00170789938961151));
#31066=CARTESIAN_POINT('',(-9.8,-1.954,-2.39295984553393E-16));
#31067=CARTESIAN_POINT('Ctrl Pts',(-7.52013030787576,-1.95318687626922,
0.00173935763946309));
#31068=CARTESIAN_POINT('Ctrl Pts',(-7.53031599220489,-1.95473250819494,
0.180522821393295));
#31069=CARTESIAN_POINT('Ctrl Pts',(-7.54050167653401,-1.93219994537477,
0.35892380617724));
#31070=CARTESIAN_POINT('Ctrl Pts',(-7.55068736086313,-1.88403259827928,
0.530111909164095));
#31071=CARTESIAN_POINT('Ctrl Pts',(-7.5877005342007,-1.70900004183546,1.15218252557468));
#31072=CARTESIAN_POINT('Ctrl Pts',(-7.62471370753826,-1.19546498257306,
1.67900839505789));
#31073=CARTESIAN_POINT('Ctrl Pts',(-7.66172688087582,-0.578068802883992,
1.86987537733102));
#31074=CARTESIAN_POINT('Ctrl Pts',(-7.69874005421339,0.0393273768050723,
2.06074235960415));
#31075=CARTESIAN_POINT('Ctrl Pts',(-7.73575322755095,0.760584676920769,
1.91565045466718));
#31076=CARTESIAN_POINT('Ctrl Pts',(-7.77276640088852,1.2561505052749,1.50089419204492));
#31077=CARTESIAN_POINT('Ctrl Pts',(-7.80977957422608,1.75171633362902,1.08613792942266));
#31078=CARTESIAN_POINT('Ctrl Pts',(-7.84679274756365,2.02159069022158,0.401717309115094));
#31079=CARTESIAN_POINT('Ctrl Pts',(-7.88380592090121,1.94246419050154,-0.239646273152209));
#31080=CARTESIAN_POINT('Ctrl Pts',(-7.92081909423877,1.8633376907815,-0.881009855419512));
#31081=CARTESIAN_POINT('Ctrl Pts',(-7.95783226757634,1.43521033474888,-1.47931639964656));
#31082=CARTESIAN_POINT('Ctrl Pts',(-7.9948454409139,0.85369952543667,-1.76119124114497));
#31083=CARTESIAN_POINT('Ctrl Pts',(-8.03185861425147,0.272188716124462,
-2.04306608264338));
#31084=CARTESIAN_POINT('Ctrl Pts',(-8.06887178758903,-0.462705546467319,
-2.00850922141314));
#31085=CARTESIAN_POINT('Ctrl Pts',(-8.1058849609266,-1.01519975043176,-1.67331017278323));
#31086=CARTESIAN_POINT('Ctrl Pts',(-8.14289813426416,-1.56769395439621,
-1.33811112415332));
#31087=CARTESIAN_POINT('Ctrl Pts',(-8.17991130760172,-1.9377880997333,-0.702269888123714));
#31088=CARTESIAN_POINT('Ctrl Pts',(-8.21692448093929,-1.95638097259055,
-0.0563112573309762));
#31089=CARTESIAN_POINT('Ctrl Pts',(-8.21799308991811,-1.95691776825236,
-0.0376617568809991));
#31090=CARTESIAN_POINT('Ctrl Pts',(-8.21906169889694,-1.95716157452165,
-0.0190038232059452));
#31091=CARTESIAN_POINT('Ctrl Pts',(-8.22013030787576,-1.95711605195191,
-0.000344670306376693));
#31092=CARTESIAN_POINT('Ctrl Pts',(-8.32186969212422,-1.95716419186761,
-0.000205378326722651));
#31093=CARTESIAN_POINT('Ctrl Pts',(-8.32123611431791,-1.95718073913763,
-0.0112676495606919));
#31094=CARTESIAN_POINT('Ctrl Pts',(-8.32060253651161,-1.95709504471771,
-0.0223296574838229));
#31095=CARTESIAN_POINT('Ctrl Pts',(-8.3199689587053,-1.9569063281076,-0.0333899075806545));
#31096=CARTESIAN_POINT('Ctrl Pts',(-8.28295578536774,-1.94588163543001,
-0.679522000462429));
#31097=CARTESIAN_POINT('Ctrl Pts',(-8.24594261203017,-1.5832612801025,-1.31965495760991));
#31098=CARTESIAN_POINT('Ctrl Pts',(-8.20892943869261,-1.03473159633512,
-1.66130303872038));
#31099=CARTESIAN_POINT('Ctrl Pts',(-8.17191626535504,-0.486201912567732,
-2.00295111983086));
#31100=CARTESIAN_POINT('Ctrl Pts',(-8.13490309201748,0.248237099639521,
-2.04611432490435));
#31101=CARTESIAN_POINT('Ctrl Pts',(-8.09788991867992,0.833009938675487,
-1.77107077921343));
#31102=CARTESIAN_POINT('Ctrl Pts',(-8.06087674534235,1.41778277771143,-1.49602723352252));
#31103=CARTESIAN_POINT('Ctrl Pts',(-8.02386357200479,1.85288944357609,-0.902776937067218));
#31104=CARTESIAN_POINT('Ctrl Pts',(-7.98685039866722,1.93952358853328,-0.262384283902055));
#31105=CARTESIAN_POINT('Ctrl Pts',(-7.94983722532966,2.02615773349047,0.378008369263136));
#31106=CARTESIAN_POINT('Ctrl Pts',(-7.91282405199209,1.76431935754017,1.06554337913819));
#31107=CARTESIAN_POINT('Ctrl Pts',(-7.87581087865453,1.2736460927936,1.48607634165523));
#31108=CARTESIAN_POINT('Ctrl Pts',(-7.83879770531696,0.782972828047029,
1.90660930417227));
#31109=CARTESIAN_POINT('Ctrl Pts',(-7.8017845319794,0.0634646745041936,
2.06014021933127));
#31110=CARTESIAN_POINT('Ctrl Pts',(-7.76477135864184,-0.556124985286757,
1.87651865529112));
#31111=CARTESIAN_POINT('Ctrl Pts',(-7.72775818530427,-1.17571464507769,
1.69289709125098));
#31112=CARTESIAN_POINT('Ctrl Pts',(-7.69074501196671,-1.69538581111674,
1.17212304801169));
#31113=CARTESIAN_POINT('Ctrl Pts',(-7.65373183862915,-1.87769342762954,
0.552145501432933));
#31114=CARTESIAN_POINT('Ctrl Pts',(-7.6431111231275,-1.93000554124126,0.374246538823964));
#31115=CARTESIAN_POINT('Ctrl Pts',(-7.63249040762586,-1.95454016061155,
0.188179459811748));
#31116=CARTESIAN_POINT('Ctrl Pts',(-7.62186969212422,-1.95297113082797,
0.00170789938961151));
#31117=CARTESIAN_POINT('Origin',(-9.8,0.,0.));
#31118=CARTESIAN_POINT('',(-6.82013030787576,-1.95113452083004,-0.00081409372327923));
#31119=CARTESIAN_POINT('',(-6.92186969212421,-1.95123700580418,-0.00092379545748507));
#31120=CARTESIAN_POINT('',(-9.8,-1.954,-2.39295984553393E-16));
#31121=CARTESIAN_POINT('Ctrl Pts',(-6.82013030787576,-1.95113452083004,
-0.00081409372327923));
#31122=CARTESIAN_POINT('Ctrl Pts',(-6.84157028551283,-1.94971586311403,
0.376507668247613));
#31123=CARTESIAN_POINT('Ctrl Pts',(-6.8630102631499,-1.84427610108052,0.754562607390817));
#31124=CARTESIAN_POINT('Ctrl Pts',(-6.88445024078697,-1.6399706578755,1.06821987854747));
#31125=CARTESIAN_POINT('Ctrl Pts',(-6.92146341412454,-1.28726540271326,
1.60970602850668));
#31126=CARTESIAN_POINT('Ctrl Pts',(-6.9584765874621,-0.639908041877813,
1.95926603940694));
#31127=CARTESIAN_POINT('Ctrl Pts',(-6.99548976079966,0.00631475279928184,
1.95718103187049));
#31128=CARTESIAN_POINT('Ctrl Pts',(-7.03250293413723,0.652537547476377,
1.95509602433404));
#31129=CARTESIAN_POINT('Ctrl Pts',(-7.0695161074748,1.29762577599512,1.60136599836088));
#31130=CARTESIAN_POINT('Ctrl Pts',(-7.10652928081236,1.64682956495479,1.05761517179331));
#31131=CARTESIAN_POINT('Ctrl Pts',(-7.14354245414993,1.99603335391445,0.513864345225741));
#31132=CARTESIAN_POINT('Ctrl Pts',(-7.18055562748749,2.04935270331504,-0.219907281936231));
#31133=CARTESIAN_POINT('Ctrl Pts',(-7.21756880082505,1.78242525341901,-0.80842914568362));
#31134=CARTESIAN_POINT('Ctrl Pts',(-7.25458197416262,1.51549780352297,-1.39695100943101));
#31135=CARTESIAN_POINT('Ctrl Pts',(-7.29159514750018,0.928323554330306,
-1.84022310976382));
#31136=CARTESIAN_POINT('Ctrl Pts',(-7.32860832083775,0.289190668548784,
-1.93570819723451));
#31137=CARTESIAN_POINT('Ctrl Pts',(-7.36562149417531,-0.349942217232729,
-2.0311932847052));
#31138=CARTESIAN_POINT('Ctrl Pts',(-7.40263466751287,-1.0410337396031,-1.77889135931378));
#31139=CARTESIAN_POINT('Ctrl Pts',(-7.43964784085044,-1.46831447397569,
-1.29408271494911));
#31140=CARTESIAN_POINT('Ctrl Pts',(-7.46647532985888,-1.77801148645166,
-0.942688943351297));
#31141=CARTESIAN_POINT('Ctrl Pts',(-7.49330281886732,-1.949115925103,-0.469148140320112));
#31142=CARTESIAN_POINT('Ctrl Pts',(-7.52013030787576,-1.95318687626922,
0.00173935763946309));
#31143=CARTESIAN_POINT('Ctrl Pts',(-7.62186969212422,-1.95297113082797,
0.00170789938961151));
#31144=CARTESIAN_POINT('Ctrl Pts',(-7.5954772342883,-1.94907209479786,-0.461673573852895));
#31145=CARTESIAN_POINT('Ctrl Pts',(-7.56908477645237,-1.7839773984951,-0.927552806989296));
#31146=CARTESIAN_POINT('Ctrl Pts',(-7.54269231861645,-1.48337286251048,
-1.27679372401467));
#31147=CARTESIAN_POINT('Ctrl Pts',(-7.50567914527889,-1.06180061389208,
-1.76657435296526));
#31148=CARTESIAN_POINT('Ctrl Pts',(-7.46866597194132,-0.373712049668737,
-2.02695456094817));
#31149=CARTESIAN_POINT('Ctrl Pts',(-7.43165279860376,0.266495499333949,
-1.93896297327993));
#31150=CARTESIAN_POINT('Ctrl Pts',(-7.39463962526619,0.906703048336636,
-1.85097138561169));
#31151=CARTESIAN_POINT('Ctrl Pts',(-7.35762645192863,1.49902958211867,-1.41460800229227));
#31152=CARTESIAN_POINT('Ctrl Pts',(-7.32061327859106,1.77283278676735,-0.829253382916534));
#31153=CARTESIAN_POINT('Ctrl Pts',(-7.2836001052535,2.04663599141603,-0.243898763540787));
#31154=CARTESIAN_POINT('Ctrl Pts',(-7.24658693191593,2.00191586693137,0.490447091891285));
#31155=CARTESIAN_POINT('Ctrl Pts',(-7.20957375857837,1.65910566639037,1.03825124640771));
#31156=CARTESIAN_POINT('Ctrl Pts',(-7.17256058524081,1.31629546584938,1.58605540092411));
#31157=CARTESIAN_POINT('Ctrl Pts',(-7.13554741190325,0.675395189252069,
1.94731785452487));
#31158=CARTESIAN_POINT('Ctrl Pts',(-7.09853423856568,0.0292411759365463,
1.95697271737387));
#31159=CARTESIAN_POINT('Ctrl Pts',(-7.06152106522812,-0.616912837378986,
1.96662758022286));
#31160=CARTESIAN_POINT('Ctrl Pts',(-7.02450789189055,-1.26832058741274,
1.62467485232006));
#31161=CARTESIAN_POINT('Ctrl Pts',(-6.98749471855299,-1.62734472261113,
1.08735753857942));
#31162=CARTESIAN_POINT('Ctrl Pts',(-6.96561970974339,-1.83953015315215,
0.769799763556305));
#31163=CARTESIAN_POINT('Ctrl Pts',(-6.9437447009338,-1.9495894566979,0.384003457058415));
#31164=CARTESIAN_POINT('Ctrl Pts',(-6.92186969212421,-1.95123700580418,
-0.00092379545748507));
#31165=CARTESIAN_POINT('Origin',(-9.8,0.,0.));
#31166=CARTESIAN_POINT('',(-6.12013030787576,-1.95615215220637,-0.00124808176673152));
#31167=CARTESIAN_POINT('',(-6.22186969212422,-1.95633073565045,-0.00114711649101067));
#31168=CARTESIAN_POINT('',(-9.8,-1.954,-2.39295984553393E-16));
#31169=CARTESIAN_POINT('Ctrl Pts',(-6.12013030787576,-1.95615215220637,
-0.00124808176673152));
#31170=CARTESIAN_POINT('Ctrl Pts',(-6.15282457882078,-1.95189699829043,
0.570376831194111));
#31171=CARTESIAN_POINT('Ctrl Pts',(-6.1855188497658,-1.68653473202121,1.14544077592247));
#31172=CARTESIAN_POINT('Ctrl Pts',(-6.21821312071081,-1.24643932389106,
1.50896868074674));
#31173=CARTESIAN_POINT('Ctrl Pts',(-6.25522629404838,-0.748207457715437,
1.9205185017209));
#31174=CARTESIAN_POINT('Ctrl Pts',(-6.29223946738595,-0.0260289193145019,
2.0609532286281));
#31175=CARTESIAN_POINT('Ctrl Pts',(-6.32925264072351,0.590122772410065,
1.86610626200643));
#31176=CARTESIAN_POINT('Ctrl Pts',(-6.36626581406107,1.20627446413461,1.67125929538477));
#31177=CARTESIAN_POINT('Ctrl Pts',(-6.40327898739864,1.71639930918277,1.14113063523426));
#31178=CARTESIAN_POINT('Ctrl Pts',(-6.4402921607362,1.88741409994161,0.517943513289022));
#31179=CARTESIAN_POINT('Ctrl Pts',(-6.47730533407376,2.05842889070045,-0.105243608656232));
#31180=CARTESIAN_POINT('Ctrl Pts',(-6.51431850741133,1.89033362716994,-0.821489192396225));
#31181=CARTESIAN_POINT('Ctrl Pts',(-6.55133168074889,1.45993339655288,-1.30353056935621));
#31182=CARTESIAN_POINT('Ctrl Pts',(-6.58834485408646,1.02953316593581,-1.78557194631621));
#31183=CARTESIAN_POINT('Ctrl Pts',(-6.62535802742402,0.336827968232211,
-2.03340911649619));
#31184=CARTESIAN_POINT('Ctrl Pts',(-6.66237120076159,-0.301675461043669,
-1.93380179538148));
#31185=CARTESIAN_POINT('Ctrl Pts',(-6.69938437409915,-0.940178890319522,
-1.83419447426678));
#31186=CARTESIAN_POINT('Ctrl Pts',(-6.73639754743671,-1.52448055116765,
-1.38714266185739));
#31187=CARTESIAN_POINT('Ctrl Pts',(-6.77341072077428,-1.7876048068472,-0.796910611143644));
#31188=CARTESIAN_POINT('Ctrl Pts',(-6.78898391647477,-1.89831364799068,
-0.548572022321792));
#31189=CARTESIAN_POINT('Ctrl Pts',(-6.80455711217527,-1.95216498059159,
-0.274886471068856));
#31190=CARTESIAN_POINT('Ctrl Pts',(-6.82013030787576,-1.95113452083004,
-0.00081409372327923));
#31191=CARTESIAN_POINT('Ctrl Pts',(-6.92186969212421,-1.95123700580418,
-0.00092379545748507));
#31192=CARTESIAN_POINT('Ctrl Pts',(-6.90673152759624,-1.9523771593765,-0.267305040402738));
#31193=CARTESIAN_POINT('Ctrl Pts',(-6.89159336306826,-1.90159831025379,
-0.5332700904781));
#31194=CARTESIAN_POINT('Ctrl Pts',(-6.87645519854029,-1.79681729382257,
-0.775915507987771));
#31195=CARTESIAN_POINT('Ctrl Pts',(-6.83944202520273,-1.54062520947259,
-1.3691893412358));
#31196=CARTESIAN_POINT('Ctrl Pts',(-6.80242885186517,-0.961600520409613,
-1.82305510815339));
#31197=CARTESIAN_POINT('Ctrl Pts',(-6.7654156785276,-0.324307740838284,
-1.93013516421731));
#31198=CARTESIAN_POINT('Ctrl Pts',(-6.72840250519004,0.312985038733054,
-2.03721522028122));
#31199=CARTESIAN_POINT('Ctrl Pts',(-6.69138933185246,1.00854590881273,-1.79750956549147));
#31200=CARTESIAN_POINT('Ctrl Pts',(-6.6543761585149,1.44456333706317,-1.32054308075455));
#31201=CARTESIAN_POINT('Ctrl Pts',(-6.61736298517734,1.8805807653136,-0.843576596017644));
#31202=CARTESIAN_POINT('Ctrl Pts',(-6.58034981183978,2.05705475173479,-0.129349281333571));
#31203=CARTESIAN_POINT('Ctrl Pts',(-6.54333663850222,1.8933518529362,0.49579837020592));
#31204=CARTESIAN_POINT('Ctrl Pts',(-6.50632346516465,1.72964895413761,1.12094602174541));
#31205=CARTESIAN_POINT('Ctrl Pts',(-6.46931029182709,1.22576917011926,1.65701401014033));
#31206=CARTESIAN_POINT('Ctrl Pts',(-6.43229711848952,0.611942252382899,
1.85906534114978));
#31207=CARTESIAN_POINT('Ctrl Pts',(-6.39528394515195,-0.00188466535346488,
2.06111667215922));
#31208=CARTESIAN_POINT('Ctrl Pts',(-6.35827077181439,-0.725658716807819,
1.92915134578318));
#31209=CARTESIAN_POINT('Ctrl Pts',(-6.32125759847683,-1.22867737075161,
1.5234661734081));
#31210=CARTESIAN_POINT('Ctrl Pts',(-6.28812829635929,-1.67891320449861,
1.1603504114159));
#31211=CARTESIAN_POINT('Ctrl Pts',(-6.25499899424176,-1.95229162706735,
0.577944956408698));
#31212=CARTESIAN_POINT('Ctrl Pts',(-6.22186969212422,-1.95633073565045,
-0.00114711649101067));
#31213=CARTESIAN_POINT('Origin',(-9.8,0.,0.));
#31214=CARTESIAN_POINT('',(-5.42013030787576,-1.9548899834603,0.00167775959234333));
#31215=CARTESIAN_POINT('',(-5.52186969212422,-1.95466140916787,0.00171701382729193));
#31216=CARTESIAN_POINT('',(-9.8,-1.954,-2.39295984553393E-16));
#31217=CARTESIAN_POINT('Ctrl Pts',(-5.42013030787576,-1.9548899834603,0.00167775959234333));
#31218=CARTESIAN_POINT('Ctrl Pts',(-5.42706569879116,-1.95599264273273,
0.123139444923241));
#31219=CARTESIAN_POINT('Ctrl Pts',(-5.43400108970656,-1.94564168131635,
0.244413763388184));
#31220=CARTESIAN_POINT('Ctrl Pts',(-5.44093648062196,-1.92315912390066,
0.363395723384609));
#31221=CARTESIAN_POINT('Ctrl Pts',(-5.47794965395953,-1.80317298254976,
0.998385151249712));
#31222=CARTESIAN_POINT('Ctrl Pts',(-5.51496282729709,-1.33765450945819,
1.56808358468529));
#31223=CARTESIAN_POINT('Ctrl Pts',(-5.55197600063466,-0.739305634289906,
1.81218780669216));
#31224=CARTESIAN_POINT('Ctrl Pts',(-5.58898917397222,-0.140956759121668,
2.05629202869902));
#31225=CARTESIAN_POINT('Ctrl Pts',(-5.62600234730978,0.590222518123277,
1.97480203927722));
#31226=CARTESIAN_POINT('Ctrl Pts',(-5.66301552064735,1.12014611452871,1.60495175931328));
#31227=CARTESIAN_POINT('Ctrl Pts',(-5.70002869398491,1.65006971093417,1.23510147934933));
#31228=CARTESIAN_POINT('Ctrl Pts',(-5.73704186732248,1.97873762650011,0.576890908843235));
#31229=CARTESIAN_POINT('Ctrl Pts',(-5.77405504066004,1.95597687368593,-0.0689342964159252));
#31230=CARTESIAN_POINT('Ctrl Pts',(-5.81106821399761,1.93321612087176,-0.714759501675086));
#31231=CARTESIAN_POINT('Ctrl Pts',(-5.84808138733517,1.55902669967746,-1.3481993416873));
#31232=CARTESIAN_POINT('Ctrl Pts',(-5.88509456067273,1.0043810130225,-1.67982625538966));
#31233=CARTESIAN_POINT('Ctrl Pts',(-5.9221077340103,0.449735326367551,-2.01145316909202));
#31234=CARTESIAN_POINT('Ctrl Pts',(-5.95912090734786,-0.285366625748073,
-2.04126715648452));
#31235=CARTESIAN_POINT('Ctrl Pts',(-5.99613408068543,-0.865046435156475,
-1.75564578791954));
#31236=CARTESIAN_POINT('Ctrl Pts',(-6.03314725402299,-1.44472624456488,
-1.47002441935456));
#31237=CARTESIAN_POINT('Ctrl Pts',(-6.07016042736056,-1.86898391126608,
-0.868967694832093));
#31238=CARTESIAN_POINT('Ctrl Pts',(-6.10717360069812,-1.94397014764153,
-0.227106875050304));
#31239=CARTESIAN_POINT('Ctrl Pts',(-6.11149250309067,-1.95271995768177,
-0.15221099392832));
#31240=CARTESIAN_POINT('Ctrl Pts',(-6.11581140548321,-1.95671425663314,
-0.0767595439546405));
#31241=CARTESIAN_POINT('Ctrl Pts',(-6.12013030787576,-1.95615215220637,
-0.00124808176673152));
#31242=CARTESIAN_POINT('Ctrl Pts',(-6.22186969212422,-1.95633073565045,
-0.00114711649101067));
#31243=CARTESIAN_POINT('Ctrl Pts',(-6.21798582090419,-1.95680425536194,
-0.0690362325279791));
#31244=CARTESIAN_POINT('Ctrl Pts',(-6.21410194968416,-1.95357604440152,
-0.136879810288365));
#31245=CARTESIAN_POINT('Ctrl Pts',(-6.21021807846414,-1.9464970931316,-0.204319184968079));
#31246=CARTESIAN_POINT('Ctrl Pts',(-6.17320490512657,-1.8790349051346,-0.847014352595043));
#31247=CARTESIAN_POINT('Ctrl Pts',(-6.136191731789,-1.46184727270742,-1.45299966947487));
#31248=CARTESIAN_POINT('Ctrl Pts',(-6.09917855845144,-0.885553085493417,
-1.7453919318276));
#31249=CARTESIAN_POINT('Ctrl Pts',(-6.06216538511387,-0.309258898279408,
-2.03778419418034));
#31250=CARTESIAN_POINT('Ctrl Pts',(-6.02515221177631,0.426141843721427,
-2.01658340200595));
#31251=CARTESIAN_POINT('Ctrl Pts',(-5.98813903843875,0.984634211045441,
-1.69147649506422));
#31252=CARTESIAN_POINT('Ctrl Pts',(-5.95112586510119,1.54312657836945,-1.36636958812248));
#31253=CARTESIAN_POINT('Ctrl Pts',(-5.91411269176361,1.92471057101666,-0.73735656641337));
#31254=CARTESIAN_POINT('Ctrl Pts',(-5.87709951842605,1.95503510249651,-0.0918423155320038));
#31255=CARTESIAN_POINT('Ctrl Pts',(-5.84008634508848,1.98535963397635,0.553671935349372));
#31256=CARTESIAN_POINT('Ctrl Pts',(-5.80307317175093,1.66442470428883,1.21568741540301));
#31257=CARTESIAN_POINT('Ctrl Pts',(-5.76605999841336,1.13886999109862,1.59171995221861));
#31258=CARTESIAN_POINT('Ctrl Pts',(-5.7290468250758,0.613315277908424,1.96775248903421));
#31259=CARTESIAN_POINT('Ctrl Pts',(-5.69203365173823,-0.11685921878447,
2.05780208261176));
#31260=CARTESIAN_POINT('Ctrl Pts',(-5.65502047840067,-0.718026514412586,
1.82072380868607));
#31261=CARTESIAN_POINT('Ctrl Pts',(-5.6180073050631,-1.31919381004069,1.58364553476039));
#31262=CARTESIAN_POINT('Ctrl Pts',(-5.58099413172554,-1.79135390460403,
1.01943939333149));
#31263=CARTESIAN_POINT('Ctrl Pts',(-5.54398095838797,-1.91877021829093,
0.385899096028444));
#31264=CARTESIAN_POINT('Ctrl Pts',(-5.53661053630006,-1.94414259055943,
0.259742406942544));
#31265=CARTESIAN_POINT('Ctrl Pts',(-5.52924011421213,-1.95584496273636,
0.130836435723866));
#31266=CARTESIAN_POINT('Ctrl Pts',(-5.52186969212422,-1.95466140916787,
0.00171701382729193));
#31267=CARTESIAN_POINT('Origin',(-9.8,0.,0.));
#31268=CARTESIAN_POINT('',(-4.72013030787576,-1.95081049221722,9.12023351157254E-5));
#31269=CARTESIAN_POINT('',(-4.82186969212422,-1.95080680701216,-3.40121725118189E-5));
#31270=CARTESIAN_POINT('',(-9.8,-1.954,-2.39295984553393E-16));
#31271=CARTESIAN_POINT('Ctrl Pts',(-4.72013030787576,-1.95081049221722,
9.12023351157254E-5));
#31272=CARTESIAN_POINT('Ctrl Pts',(-4.73831999209911,-1.95094405902827,
0.3203439412756));
#31273=CARTESIAN_POINT('Ctrl Pts',(-4.75650967632245,-1.8764768769041,0.640538180196498));
#31274=CARTESIAN_POINT('Ctrl Pts',(-4.7746993605458,-1.72706848364466,0.9207778887538));
#31275=CARTESIAN_POINT('Ctrl Pts',(-4.81171253388337,-1.42304568204481,
1.49102203271679));
#31276=CARTESIAN_POINT('Ctrl Pts',(-4.84872570722094,-0.808721983960032,
1.89583081204337));
#31277=CARTESIAN_POINT('Ctrl Pts',(-4.8857388805585,-0.164790516675161,
1.9502414089621));
#31278=CARTESIAN_POINT('Ctrl Pts',(-4.92275205389606,0.479140950609711,
2.00465200588084));
#31279=CARTESIAN_POINT('Ctrl Pts',(-4.95976522723362,1.15268018709468,1.70866442039174));
#31280=CARTESIAN_POINT('Ctrl Pts',(-4.99677840057119,1.54807765417753,1.19751953815074));
#31281=CARTESIAN_POINT('Ctrl Pts',(-5.03379157390875,1.94347512126036,0.686374655909763));
#31282=CARTESIAN_POINT('Ctrl Pts',(-5.07080474724632,2.0607308189411,-0.0399275230830835));
#31283=CARTESIAN_POINT('Ctrl Pts',(-5.10781792058388,1.84626897181572,-0.649529330613395));
#31284=CARTESIAN_POINT('Ctrl Pts',(-5.14483109392145,1.63180712469032,-1.25913113814376));
#31285=CARTESIAN_POINT('Ctrl Pts',(-5.18184426725901,1.08562773275873,-1.75203257421157));
#31286=CARTESIAN_POINT('Ctrl Pts',(-5.21885744059658,0.457287832576391,
-1.90302004871051));
#31287=CARTESIAN_POINT('Ctrl Pts',(-5.25587061393414,-0.171052067605934,
-2.05400752320944));
#31288=CARTESIAN_POINT('Ctrl Pts',(-5.2928837872717,-0.881552476039011,
-1.86308103613953));
#31289=CARTESIAN_POINT('Ctrl Pts',(-5.32989696060927,-1.34957577545042,
-1.41747758145727));
#31290=CARTESIAN_POINT('Ctrl Pts',(-5.35997474303143,-1.72990260773292,
-1.05536964668869));
#31291=CARTESIAN_POINT('Ctrl Pts',(-5.39005252545359,-1.95010791045442,
-0.525083916652837));
#31292=CARTESIAN_POINT('Ctrl Pts',(-5.42013030787576,-1.9548899834603,0.00167775959234333));
#31293=CARTESIAN_POINT('Ctrl Pts',(-5.52186969212422,-1.95466140916787,
0.00171701382729193));
#31294=CARTESIAN_POINT('Ctrl Pts',(-5.49222694087457,-1.94990133116922,
-0.517582269052512));
#31295=CARTESIAN_POINT('Ctrl Pts',(-5.46258418962493,-1.73670755972907,
-1.04033418033024));
#31296=CARTESIAN_POINT('Ctrl Pts',(-5.43294143837528,-1.36608778935965,
-1.40157105231175));
#31297=CARTESIAN_POINT('Ctrl Pts',(-5.39592826503772,-0.903316513931034,
-1.85262645017167));
#31298=CARTESIAN_POINT('Ctrl Pts',(-5.35891509170015,-0.195101430263383,
-2.05186279271431));
#31299=CARTESIAN_POINT('Ctrl Pts',(-5.32190191836259,0.43496404135903,-1.90824619628611));
#31300=CARTESIAN_POINT('Ctrl Pts',(-5.28488874502503,1.06502951298146,-1.76462959985791));
#31301=CARTESIAN_POINT('Ctrl Pts',(-5.24787557168746,1.61694537255866,-1.2781600644588));
#31302=CARTESIAN_POINT('Ctrl Pts',(-5.2108623983499,1.83853351088562,-0.671112354428362));
#31303=CARTESIAN_POINT('Ctrl Pts',(-5.17384922501233,2.06012164921258,-0.0640646443979367));
#31304=CARTESIAN_POINT('Ctrl Pts',(-5.13683605167477,1.95138206628935,0.66356124026384));
#31305=CARTESIAN_POINT('Ctrl Pts',(-5.0998228783372,1.56199940505829,1.17930281162784));
#31306=CARTESIAN_POINT('Ctrl Pts',(-5.06280970499964,1.17261674382722,1.69504438299186));
#31307=CARTESIAN_POINT('Ctrl Pts',(-5.02579653166207,0.502591004288316,
1.99890164105808));
#31308=CARTESIAN_POINT('Ctrl Pts',(-4.98878335832451,-0.141933641066262,
1.9520379362219));
#31309=CARTESIAN_POINT('Ctrl Pts',(-4.95177018498695,-0.78645828642084,
1.90517423138573));
#31310=CARTESIAN_POINT('Ctrl Pts',(-4.91475701164938,-1.40548183759107,
1.50758956364717));
#31311=CARTESIAN_POINT('Ctrl Pts',(-4.87774383831182,-1.71616373839683,
0.940945952713336));
#31312=CARTESIAN_POINT('Ctrl Pts',(-4.85911912291595,-1.87249624002759,
0.655815686030199));
#31313=CARTESIAN_POINT('Ctrl Pts',(-4.84049440752008,-1.95075610609356,
0.32787940450784));
#31314=CARTESIAN_POINT('Ctrl Pts',(-4.82186969212422,-1.95080709904697,
-3.40090619142402E-5));
#31315=CARTESIAN_POINT('Origin',(-9.8,0.,0.));
#31316=CARTESIAN_POINT('',(-4.02013030787576,-1.9545563311611,-0.00173175715877188));
#31317=CARTESIAN_POINT('',(-4.12186969212422,-1.95478583214071,-0.00169688232281055));
#31318=CARTESIAN_POINT('',(-9.8,-1.954,-2.39295984553393E-16));
#31319=CARTESIAN_POINT('Ctrl Pts',(-4.02013030787576,-1.9545563311611,-0.00173175715877189));
#31320=CARTESIAN_POINT('Ctrl Pts',(-4.04957428540706,-1.94981507723237,
0.514156697093934));
#31321=CARTESIAN_POINT('Ctrl Pts',(-4.07901826293835,-1.73977891611187,
1.03345910076901));
#31322=CARTESIAN_POINT('Ctrl Pts',(-4.10846224046964,-1.37357022290306,
1.39423897175874));
#31323=CARTESIAN_POINT('Ctrl Pts',(-4.14547541380721,-0.913219856684524,
1.84776492243762));
#31324=CARTESIAN_POINT('Ctrl Pts',(-4.18248858714477,-0.206081319881922,
2.05078916635255));
#31325=CARTESIAN_POINT('Ctrl Pts',(-4.21950176048234,0.424743856605548,
1.91054707450309));
#31326=CARTESIAN_POINT('Ctrl Pts',(-4.2565149338199,1.055569033093,1.77030498265363));
#31327=CARTESIAN_POINT('Ctrl Pts',(-4.29352810715747,1.61008084926532,1.28679655503981));
#31328=CARTESIAN_POINT('Ctrl Pts',(-4.33054128049503,1.83491506688298,0.68094358425817));
#31329=CARTESIAN_POINT('Ctrl Pts',(-4.3675544538326,2.05974928450064,0.0750906134765319));
#31330=CARTESIAN_POINT('Ctrl Pts',(-4.40456762717016,1.95490590356363,-0.653106900472918));
#31331=CARTESIAN_POINT('Ctrl Pts',(-4.44158080050773,1.56828933759538,-1.17092528420956));
#31332=CARTESIAN_POINT('Ctrl Pts',(-4.47859397384529,1.18167277162715,-1.68874366794618));
#31333=CARTESIAN_POINT('Ctrl Pts',(-4.51560714718285,0.513283020627696,
-1.99618292147001));
#31334=CARTESIAN_POINT('Ctrl Pts',(-4.55262032052042,-0.131483249055789,
-1.95276973113429));
#31335=CARTESIAN_POINT('Ctrl Pts',(-4.58963349385798,-0.776249518739292,
-1.90935654079856));
#31336=CARTESIAN_POINT('Ctrl Pts',(-4.62664666719555,-1.39739230710683,
-1.51509090660327));
#31337=CARTESIAN_POINT('Ctrl Pts',(-4.66365984053311,-1.71110274873313,
-0.950118335205926));
#31338=CARTESIAN_POINT('Ctrl Pts',(-4.68248332964733,-1.87064392152352,
-0.662794820668581));
#31339=CARTESIAN_POINT('Ctrl Pts',(-4.70130681876154,-1.95067227137827,
-0.331320485257933));
#31340=CARTESIAN_POINT('Ctrl Pts',(-4.72013030787576,-1.95081049221722,
9.12023351157254E-5));
#31341=CARTESIAN_POINT('Ctrl Pts',(-4.82186969212422,-1.95080709904697,
-3.40090619142402E-5));
#31342=CARTESIAN_POINT('Ctrl Pts',(-4.80348123418252,-1.95085744514672,
-0.323787789228885));
#31343=CARTESIAN_POINT('Ctrl Pts',(-4.78509277624082,-1.87467051708849,
-0.647519277930666));
#31344=CARTESIAN_POINT('Ctrl Pts',(-4.76670431829912,-1.72211519641974,
-0.930008878009234));
#31345=CARTESIAN_POINT('Ctrl Pts',(-4.72969114496156,-1.41504450319559,
-1.49861754366889));
#31346=CARTESIAN_POINT('Ctrl Pts',(-4.69267797162399,-0.798562866305986,
-1.9001323208591));
#31347=CARTESIAN_POINT('Ctrl Pts',(-4.65566479828643,-0.154349405589037,
-1.9510954676566));
#31348=CARTESIAN_POINT('Ctrl Pts',(-4.61865162494886,0.489864055127912,
-2.00205861445409));
#31349=CARTESIAN_POINT('Ctrl Pts',(-4.5816384516113,1.16180933967221,-1.70247013085888));
#31350=CARTESIAN_POINT('Ctrl Pts',(-4.54462527827373,1.55446520847415,-1.18921620345471));
#31351=CARTESIAN_POINT('Ctrl Pts',(-4.50761210493617,1.94712107727608,-0.675962276050554));
#31352=CARTESIAN_POINT('Ctrl Pts',(-4.47059893159861,2.06048753033567,0.0509570951625461));
#31353=CARTESIAN_POINT('Ctrl Pts',(-4.43358575826104,1.84276584274993,0.659402238174801));
#31354=CARTESIAN_POINT('Ctrl Pts',(-4.39657258492348,1.62504415516418,1.26784738118709));
#31355=CARTESIAN_POINT('Ctrl Pts',(-4.35955941158591,1.07623432693307,1.75781829599852));
#31356=CARTESIAN_POINT('Ctrl Pts',(-4.32254623824835,0.447095277907961,
1.90544038883094));
#31357=CARTESIAN_POINT('Ctrl Pts',(-4.28553306491079,-0.182043771117111,
2.05306248166334));
#31358=CARTESIAN_POINT('Ctrl Pts',(-4.24851989157322,-0.891512040936168,
1.85833575251678));
#31359=CARTESIAN_POINT('Ctrl Pts',(-4.21150671823566,-1.35714351290836,
1.41023357933592));
#31360=CARTESIAN_POINT('Ctrl Pts',(-4.18162770953184,-1.73302608522773,
1.0485015924414));
#31361=CARTESIAN_POINT('Ctrl Pts',(-4.15174870082803,-1.95001045891771,
0.52165547187433));
#31362=CARTESIAN_POINT('Ctrl Pts',(-4.12186969212422,-1.95478583214071,
-0.00169688232281055));
#31363=CARTESIAN_POINT('Origin',(-9.8,0.,0.));
#31364=CARTESIAN_POINT('',(-3.32013030787577,-1.95640828841667,0.00109851928146481));
#31365=CARTESIAN_POINT('',(-3.42186969212422,-1.95623519870294,0.0012028883663872));
#31366=CARTESIAN_POINT('',(-9.8,-1.954,-2.39295984553393E-16));
#31367=CARTESIAN_POINT('Ctrl Pts',(-3.32013030787577,-1.95640828841667,
0.00109851928146481));
#31368=CARTESIAN_POINT('Ctrl Pts',(-3.32381540537744,-1.95684244368226,
0.0655064059659674));
#31369=CARTESIAN_POINT('Ctrl Pts',(-3.32750050287912,-1.95393695034547,
0.12987464599085));
#31370=CARTESIAN_POINT('Ctrl Pts',(-3.3311856003808,-1.94756288843026,0.193897558538627));
#31371=CARTESIAN_POINT('Ctrl Pts',(-3.36819877371836,-1.8835417170977,0.836944630869362));
#31372=CARTESIAN_POINT('Ctrl Pts',(-3.40521194705592,-1.46960361082938,
1.44515429704656));
#31373=CARTESIAN_POINT('Ctrl Pts',(-3.44222512039348,-0.894882705104787,
1.74062701683428));
#31374=CARTESIAN_POINT('Ctrl Pts',(-3.47923829373105,-0.320161799380146,
2.03609973662201));
#31375=CARTESIAN_POINT('Ctrl Pts',(-3.51625146706862,0.415341905800802,
2.0188355100202));
#31376=CARTESIAN_POINT('Ctrl Pts',(-3.55326464040618,0.975566435643367,
1.69672260468841));
#31377=CARTESIAN_POINT('Ctrl Pts',(-3.59027781374375,1.53579096548592,1.37460969935663));
#31378=CARTESIAN_POINT('Ctrl Pts',(-3.62729098708131,1.92073631999009,0.747648115294896));
#31379=CARTESIAN_POINT('Ctrl Pts',(-3.66430416041887,1.95451555921865,0.102305407415552));
#31380=CARTESIAN_POINT('Ctrl Pts',(-3.70131733375644,1.98829479844721,-0.543037300463793));
#31381=CARTESIAN_POINT('Ctrl Pts',(-3.738330507094,1.67090792240016,-1.20676113216074));
#31382=CARTESIAN_POINT('Ctrl Pts',(-3.77534368043157,1.14737345319091,-1.58560134539902));
#31383=CARTESIAN_POINT('Ctrl Pts',(-3.81235685376913,0.623838983981661,
-1.9644415586373));
#31384=CARTESIAN_POINT('Ctrl Pts',(-3.8493700271067,-0.105843078389784,
-2.05839815341691));
#31385=CARTESIAN_POINT('Ctrl Pts',(-3.88638320044426,-0.708270749513731,
-1.82454104174156));
#31386=CARTESIAN_POINT('Ctrl Pts',(-3.92339637378182,-1.31069842063764,
-1.59068393006623));
#31387=CARTESIAN_POINT('Ctrl Pts',(-3.96040954711939,-1.78587170051407,
-1.02901311193597));
#31388=CARTESIAN_POINT('Ctrl Pts',(-3.99742272045695,-1.91667724263507,
-0.396163874149472));
#31389=CARTESIAN_POINT('Ctrl Pts',(-4.00499191626322,-1.94342698256765,
-0.266746173241493));
#31390=CARTESIAN_POINT('Ctrl Pts',(-4.01256111206949,-1.95577517054229,
-0.13435177156693));
#31391=CARTESIAN_POINT('Ctrl Pts',(-4.02013030787576,-1.9545563311611,-0.00173175715877189));
#31392=CARTESIAN_POINT('Ctrl Pts',(-4.12186969212422,-1.95478583214071,
-0.00169688232281055));
#31393=CARTESIAN_POINT('Ctrl Pts',(-4.11473552749047,-1.95592604060941,
-0.126656913404005));
#31394=CARTESIAN_POINT('Ctrl Pts',(-4.10760136285672,-1.94496813473903,
-0.251417763560148));
#31395=CARTESIAN_POINT('Ctrl Pts',(-4.10046719822296,-1.9211864330455,-0.373684295091019));
#31396=CARTESIAN_POINT('Ctrl Pts',(-4.0634540248854,-1.79780320708513,-1.00802237912193));
#31397=CARTESIAN_POINT('Ctrl Pts',(-4.02644085154783,-1.32924208103907,
-1.57522092996857));
#31398=CARTESIAN_POINT('Ctrl Pts',(-3.98942767821027,-0.729595215447372,
-1.81611896210353));
#31399=CARTESIAN_POINT('Ctrl Pts',(-3.95241450487271,-0.129948349855691,
-2.05701699423849));
#31400=CARTESIAN_POINT('Ctrl Pts',(-3.91540133153514,0.600784255281619,
-1.97161450766178));
#31401=CARTESIAN_POINT('Ctrl Pts',(-3.87838815819758,1.12872060780878,-1.5989330981701));
#31402=CARTESIAN_POINT('Ctrl Pts',(-3.84137498486002,1.65665696033596,-1.22625168867841));
#31403=CARTESIAN_POINT('Ctrl Pts',(-3.80436181152245,1.98179706025298,-0.566291356271734));
#31404=CARTESIAN_POINT('Ctrl Pts',(-3.76734863818489,1.95557982854599,0.0794027524685451));
#31405=CARTESIAN_POINT('Ctrl Pts',(-3.73033546484732,1.92936259683899,0.725096861208825));
#31406=CARTESIAN_POINT('Ctrl Pts',(-3.69332229150975,1.55178803350799,1.3565247462827));
#31407=CARTESIAN_POINT('Ctrl Pts',(-3.65630911817219,0.995375260466554,
1.68517813710198));
#31408=CARTESIAN_POINT('Ctrl Pts',(-3.61929594483462,0.438962487425118,
2.01383152792126));
#31409=CARTESIAN_POINT('Ctrl Pts',(-3.58228277149706,-0.296288495326749,
2.03971042448594));
#31410=CARTESIAN_POINT('Ctrl Pts',(-3.5452695981595,-0.874431185429084,
1.7509903954239));
#31411=CARTESIAN_POINT('Ctrl Pts',(-3.50825642482194,-1.45257387553142,
1.46227036636187));
#31412=CARTESIAN_POINT('Ctrl Pts',(-3.47124325148437,-1.87360827298422,
0.858951411673132));
#31413=CARTESIAN_POINT('Ctrl Pts',(-3.4342300781468,-1.94515784716871,0.216698436799811));
#31414=CARTESIAN_POINT('Ctrl Pts',(-3.43010994947261,-1.95312240209988,
0.145205920507576));
#31415=CARTESIAN_POINT('Ctrl Pts',(-3.42598982079841,-1.95675646506019,
0.0732309699275622));
#31416=CARTESIAN_POINT('Ctrl Pts',(-3.42186969212422,-1.95623519870294,
0.0012028883663872));
#31417=CARTESIAN_POINT('Origin',(-9.8,0.,0.));
#31418=CARTESIAN_POINT('',(-2.62013030787576,-1.95128826882871,0.000972458038924484));
#31419=CARTESIAN_POINT('',(-2.72186969212422,-1.95117967829402,0.000864741168076029));
#31420=CARTESIAN_POINT('',(-9.8,-1.954,-2.39295984553393E-16));
#31421=CARTESIAN_POINT('Ctrl Pts',(-2.62013030787576,-1.95128826882871,
0.000972458038924484));
#31422=CARTESIAN_POINT('Ctrl Pts',(-2.63506969868539,-1.95247456011625,
0.263838687422591));
#31423=CARTESIAN_POINT('Ctrl Pts',(-2.65000908949501,-1.90306670254861,
0.526277490250255));
#31424=CARTESIAN_POINT('Ctrl Pts',(-2.66494848030464,-1.8009447216931,0.766286875754349));
#31425=CARTESIAN_POINT('Ctrl Pts',(-2.7019616536422,-1.54793182262993,1.3609235046176));
#31426=CARTESIAN_POINT('Ctrl Pts',(-2.73897482697977,-0.97134474800472,
1.81788203573128));
#31427=CARTESIAN_POINT('Ctrl Pts',(-2.77598800031733,-0.334634231049586,
1.92837169641715));
#31428=CARTESIAN_POINT('Ctrl Pts',(-2.81300117365489,0.302076285905531,
2.03886135710302));
#31429=CARTESIAN_POINT('Ctrl Pts',(-2.85001434699246,0.998910245190565,
1.80288214736111));
#31430=CARTESIAN_POINT('Ctrl Pts',(-2.88702752033002,1.4374744217618,1.32825628340228));
#31431=CARTESIAN_POINT('Ctrl Pts',(-2.92404069366758,1.87603859833305,0.85363041944343));
#31432=CARTESIAN_POINT('Ctrl Pts',(-2.96105386700515,2.05633299219049,0.140357901267651));
#31433=CARTESIAN_POINT('Ctrl Pts',(-2.99806704034272,1.89597856231094,-0.485657038177132));
#31434=CARTESIAN_POINT('Ctrl Pts',(-3.03508021368028,1.7356241324314,-1.11167197762192));
#31435=CARTESIAN_POINT('Ctrl Pts',(-3.07209338701784,1.23462087881487,-1.6504293383357));
#31436=CARTESIAN_POINT('Ctrl Pts',(-3.10910656035541,0.621884225714157,
-1.85576331397781));
#31437=CARTESIAN_POINT('Ctrl Pts',(-3.14611973369297,0.00914757261343817,
-2.06109728961992));
#31438=CARTESIAN_POINT('Ctrl Pts',(-3.18313290703054,-0.715322479971475,
-1.93300788019034));
#31439=CARTESIAN_POINT('Ctrl Pts',(-3.2201460803681,-1.22050538806554,-1.5300209362334));
#31440=CARTESIAN_POINT('Ctrl Pts',(-3.25347415620399,-1.67539138550219,
-1.16715609061264));
#31441=CARTESIAN_POINT('Ctrl Pts',(-3.28680223203988,-1.95248178182908,
-0.581407352238547));
#31442=CARTESIAN_POINT('Ctrl Pts',(-3.32013030787577,-1.95640828841667,
0.00109851928146481));
#31443=CARTESIAN_POINT('Ctrl Pts',(-3.42186969212422,-1.95623519870294,
0.0012028883663872));
#31444=CARTESIAN_POINT('Ctrl Pts',(-3.38897664746085,-1.9520736690697,-0.573833255200393));
#31445=CARTESIAN_POINT('Ctrl Pts',(-3.35608360279748,-1.68306698074724,
-1.15225576891058));
#31446=CARTESIAN_POINT('Ctrl Pts',(-3.32319055813411,-1.23834461947855,
-1.51561864145381));
#31447=CARTESIAN_POINT('Ctrl Pts',(-3.28617738479655,-0.737917066687742,
-1.92449574977619));
#31448=CARTESIAN_POINT('Ctrl Pts',(-3.24916421145898,-0.0149972101899386,
-2.06106297136309));
#31449=CARTESIAN_POINT('Ctrl Pts',(-3.21215103812142,0.60010271245489,-1.86292082425223));
#31450=CARTESIAN_POINT('Ctrl Pts',(-3.17513786478386,1.21520263509974,-1.66477867714137));
#31451=CARTESIAN_POINT('Ctrl Pts',(-3.13812469144629,1.7224826238916,-1.13192716133273));
#31452=CARTESIAN_POINT('Ctrl Pts',(-3.10111151810873,1.89015932601566,-0.507833619577597));
#31453=CARTESIAN_POINT('Ctrl Pts',(-3.06409834477116,2.05783602813972,0.116259922177535));
#31454=CARTESIAN_POINT('Ctrl Pts',(-3.0270851714336,1.88590944359597,0.831595489879161));
#31455=CARTESIAN_POINT('Ctrl Pts',(-2.99007199809603,1.4529352439555,1.31132621409805));
#31456=CARTESIAN_POINT('Ctrl Pts',(-2.95305882475847,1.01996104431503,1.79105693831693));
#31457=CARTESIAN_POINT('Ctrl Pts',(-2.91604565142091,0.325939229577842,
2.03518281905308));
#31458=CARTESIAN_POINT('Ctrl Pts',(-2.87903247808334,-0.312021883881085,
1.93215931200737));
#31459=CARTESIAN_POINT('Ctrl Pts',(-2.84201930474578,-0.949982997340013,
1.82913580496166));
#31460=CARTESIAN_POINT('Ctrl Pts',(-2.80500613140821,-1.53188340952068,
1.3789629101341));
#31461=CARTESIAN_POINT('Ctrl Pts',(-2.76799295807065,-1.79184464801151,
0.787330947038803));
#31462=CARTESIAN_POINT('Ctrl Pts',(-2.7526185360885,-1.89982657496242,0.541580619829814));
#31463=CARTESIAN_POINT('Ctrl Pts',(-2.73724411410636,-1.95226173617185,
0.271423217094667));
#31464=CARTESIAN_POINT('Ctrl Pts',(-2.72186969212422,-1.95117967829402,
0.000864741168076028));
#31465=CARTESIAN_POINT('Origin',(-9.8,0.,0.));
#31466=CARTESIAN_POINT('',(-1.92013030787577,-1.95287461439042,-0.00169055101731763));
#31467=CARTESIAN_POINT('',(-2.02186969212423,-1.95308757850967,-0.00172609056776994));
#31468=CARTESIAN_POINT('',(-9.8,-1.954,-2.39295984553393E-16));
#31469=CARTESIAN_POINT('Ctrl Pts',(-1.92013030787577,-1.95287461439042,
-0.00169055101731763));
#31470=CARTESIAN_POINT('Ctrl Pts',(-1.94632399199334,-1.94905843635623,
0.458258638527069));
#31471=CARTESIAN_POINT('Ctrl Pts',(-1.97251767611091,-1.78666677165177,
0.920633103135576));
#31472=CARTESIAN_POINT('Ctrl Pts',(-1.99871136022848,-1.49018573369743,
1.26883564400827));
#31473=CARTESIAN_POINT('Ctrl Pts',(-2.03572453356604,-1.07124107513584,
1.7608657434801));
#31474=CARTESIAN_POINT('Ctrl Pts',(-2.07273770690361,-0.384556063773794,
2.02492527078759));
#31475=CARTESIAN_POINT('Ctrl Pts',(-2.10975088024117,0.256113305508671,
1.94036168303737));
#31476=CARTESIAN_POINT('Ctrl Pts',(-2.14676405357874,0.896782674791118,
1.85579809528716));
#31477=CARTESIAN_POINT('Ctrl Pts',(-2.1837772269163,1.49143640199399,1.42261139247926));
#31478=CARTESIAN_POINT('Ctrl Pts',(-2.22079040025386,1.76836882853465,0.838730682929604));
#31479=CARTESIAN_POINT('Ctrl Pts',(-2.25780357359143,2.04530125507533,0.254849973379925));
#31480=CARTESIAN_POINT('Ctrl Pts',(-2.29481674692899,2.00451238095378,-0.479724742911528));
#31481=CARTESIAN_POINT('Ctrl Pts',(-2.33182992026656,1.66463922482719,-1.0293559690438));
#31482=CARTESIAN_POINT('Ctrl Pts',(-2.36884309360412,1.32476606870059,-1.57898719517607));
#31483=CARTESIAN_POINT('Ctrl Pts',(-2.40585626694168,0.685808630568944,
-1.94367493114915));
#31484=CARTESIAN_POINT('Ctrl Pts',(-2.44286944027925,0.0397155348038179,
-1.95678822233774));
#31485=CARTESIAN_POINT('Ctrl Pts',(-2.47988261361681,-0.606377560961308,
-1.96990151352634));
#31486=CARTESIAN_POINT('Ctrl Pts',(-2.51689578695438,-1.25960631435991,
-1.63144035993043));
#31487=CARTESIAN_POINT('Ctrl Pts',(-2.55390896029194,-1.62150132930865,
-1.09605241982608));
#31488=CARTESIAN_POINT('Ctrl Pts',(-2.57598274281988,-1.83732697022491,
-0.776759695309758));
#31489=CARTESIAN_POINT('Ctrl Pts',(-2.59805652534782,-1.94953545733662,
-0.387427046016949));
#31490=CARTESIAN_POINT('Ctrl Pts',(-2.62013030787576,-1.95128826882871,
0.000972458038924484));
#31491=CARTESIAN_POINT('Ctrl Pts',(-2.72186969212422,-1.95117967829402,
0.000864741168076028));
#31492=CARTESIAN_POINT('Ctrl Pts',(-2.7002309407688,-1.94965673444626,-0.379933157736906));
#31493=CARTESIAN_POINT('Ctrl Pts',(-2.67859218941338,-1.84212049455112,
-0.761525550296575));
#31494=CARTESIAN_POINT('Ctrl Pts',(-2.65695343805795,-1.63422943147789,
-1.07698255705823));
#31495=CARTESIAN_POINT('Ctrl Pts',(-2.61994026472039,-1.27863091165242,
-1.61657306669692));
#31496=CARTESIAN_POINT('Ctrl Pts',(-2.58292709138282,-0.629411807200471,
-1.9626630546113));
#31497=CARTESIAN_POINT('Ctrl Pts',(-2.54591391804526,0.0167905529389563,
-1.95711914322188));
#31498=CARTESIAN_POINT('Ctrl Pts',(-2.5089007447077,0.662992913078401,-1.95157523183247));
#31499=CARTESIAN_POINT('Ctrl Pts',(-2.47188757137013,1.30617852890533,-1.59439742113925));
#31500=CARTESIAN_POINT('Ctrl Pts',(-2.43487439803257,1.65246685804866,-1.04878527110899));
#31501=CARTESIAN_POINT('Ctrl Pts',(-2.397861224695,1.998755187192,-0.503173121078729));
#31502=CARTESIAN_POINT('Ctrl Pts',(-2.36084805135744,2.04814622965175,0.230873368288563));
#31503=CARTESIAN_POINT('Ctrl Pts',(-2.32383487801987,1.77807252324082,0.817958046205187));
#31504=CARTESIAN_POINT('Ctrl Pts',(-2.28682170468231,1.50799881682989,1.40504272412181));
#31505=CARTESIAN_POINT('Ctrl Pts',(-2.24980853134475,0.918460361548285,
1.84516559058777));
#31506=CARTESIAN_POINT('Ctrl Pts',(-2.21279535800718,0.27882556111846,1.93722832225799));
#31507=CARTESIAN_POINT('Ctrl Pts',(-2.17578218466962,-0.360809239311365,
2.02929105392822));
#31508=CARTESIAN_POINT('Ctrl Pts',(-2.13876901133205,-1.05054038488941,
1.77329365080272));
#31509=CARTESIAN_POINT('Ctrl Pts',(-2.10175583799449,-1.47522003017977,
1.28620492833718));
#31510=CARTESIAN_POINT('Ctrl Pts',(-2.0751271227044,-1.78075107073109,0.935774372349613));
#31511=CARTESIAN_POINT('Ctrl Pts',(-2.04849840741431,-1.9490935021035,0.465732734518825));
#31512=CARTESIAN_POINT('Ctrl Pts',(-2.02186969212423,-1.95308757850967,
-0.00172609056776994));
#31513=CARTESIAN_POINT('Origin',(-9.8,0.,0.));
#31514=CARTESIAN_POINT('',(-1.22013030787577,-1.95717923962325,0.000142060037185308));
#31515=CARTESIAN_POINT('',(-1.32186969212423,-1.95714098413823,0.000281429570410231));
#31516=CARTESIAN_POINT('',(-9.8,-1.954,-2.39295984553393E-16));
#31517=CARTESIAN_POINT('Ctrl Pts',(-1.22013030787577,-1.95717923962325,
0.000142060037185308));
#31518=CARTESIAN_POINT('Ctrl Pts',(-1.22056511196372,-1.95718716035574,
0.00773360395988979));
#31519=CARTESIAN_POINT('Ctrl Pts',(-1.22099991605168,-1.95714681216893,
0.0153250610537409));
#31520=CARTESIAN_POINT('Ctrl Pts',(-1.22143472013963,-1.95705794020611,
0.0229159496253129));
#31521=CARTESIAN_POINT('Ctrl Pts',(-1.25844789347719,-1.94949261721163,
0.669098638040081));
#31522=CARTESIAN_POINT('Ctrl Pts',(-1.29546106681476,-1.59030209252517,
1.31116155718884));
#31523=CARTESIAN_POINT('Ctrl Pts',(-1.33247424015232,-1.04360853567726,
1.65574034778633));
#31524=CARTESIAN_POINT('Ctrl Pts',(-1.36948741348988,-0.496914978829352,
2.00031913838382));
#31525=CARTESIAN_POINT('Ctrl Pts',(-1.40650058682745,0.237281610179996,
2.04741380043005));
#31526=CARTESIAN_POINT('Ctrl Pts',(-1.44351376016501,0.823518058849043,
1.77550443541525));
#31527=CARTESIAN_POINT('Ctrl Pts',(-1.48052693350258,1.40975450751809,1.50359507040046));
#31528=CARTESIAN_POINT('Ctrl Pts',(-1.51754010684014,1.84803081584683,0.91268167832465));
#31529=CARTESIAN_POINT('Ctrl Pts',(-1.55455328017771,1.93809156072536,0.27276177482246));
#31530=CARTESIAN_POINT('Ctrl Pts',(-1.59156645351527,2.02815230560389,-0.367158128679712));
#31531=CARTESIAN_POINT('Ctrl Pts',(-1.62857962685283,1.76999748703222,-1.05608454360826));
#31532=CARTESIAN_POINT('Ctrl Pts',(-1.6655928001904,1.28158209960214,-1.47923777903418));
#31533=CARTESIAN_POINT('Ctrl Pts',(-1.70260597352796,0.793166712172057,
-1.90239101446009));
#31534=CARTESIAN_POINT('Ctrl Pts',(-1.73961914686552,0.0744907558835552,
-2.05977107038337));
#31535=CARTESIAN_POINT('Ctrl Pts',(-1.77663232020309,-0.546072856156742,
-1.87946854374991));
#31536=CARTESIAN_POINT('Ctrl Pts',(-1.81364549354065,-1.16663646819707,
-1.69916601711645));
#31537=CARTESIAN_POINT('Ctrl Pts',(-1.85065866687822,-1.68908773598919,
-1.18118090792619));
#31538=CARTESIAN_POINT('Ctrl Pts',(-1.88767184021578,-1.87471121700467,
-0.562188017512963));
#31539=CARTESIAN_POINT('Ctrl Pts',(-1.89849132943578,-1.9289716618876,-0.381247387429709));
#31540=CARTESIAN_POINT('Ctrl Pts',(-1.90931081865577,-1.95445091411662,
-0.191675864869495));
#31541=CARTESIAN_POINT('Ctrl Pts',(-1.92013030787577,-1.95287461439042,
-0.00169055101731763));
#31542=CARTESIAN_POINT('Ctrl Pts',(-2.02186969212423,-1.95308757850967,
-0.00172609056776994));
#31543=CARTESIAN_POINT('Ctrl Pts',(-2.01148523407675,-1.95464515717716,
-0.184022025807307));
#31544=CARTESIAN_POINT('Ctrl Pts',(-2.00110077602927,-1.93120891772511,
-0.365925171280384));
#31545=CARTESIAN_POINT('Ctrl Pts',(-1.9907163179818,-1.8811681159904,-0.540188658624532));
#31546=CARTESIAN_POINT('Ctrl Pts',(-1.95370314464423,-1.70280841150797,
-1.16131348131528));
#31547=CARTESIAN_POINT('Ctrl Pts',(-1.91668997130667,-1.18646085754039,
-1.6853830848912));
#31548=CARTESIAN_POINT('Ctrl Pts',(-1.8796767979691,-0.568051918879918,
-1.87294268440246));
#31549=CARTESIAN_POINT('Ctrl Pts',(-1.84266362463154,0.05035701978055,-2.06050228391373));
#31550=CARTESIAN_POINT('Ctrl Pts',(-1.80565045129397,0.770827343133897,
-1.91155187936033));
#31551=CARTESIAN_POINT('Ctrl Pts',(-1.76863727795641,1.2641660664822,-1.49414904342711));
#31552=CARTESIAN_POINT('Ctrl Pts',(-1.73162410461884,1.75750478983048,-1.07674620749391));
#31553=CARTESIAN_POINT('Ctrl Pts',(-1.69461093128128,2.02371191317375,-0.39089094018093));
#31554=CARTESIAN_POINT('Ctrl Pts',(-1.65759775794372,1.94115361144894,0.250039929439042));
#31555=CARTESIAN_POINT('Ctrl Pts',(-1.62058458460615,1.85859530972413,0.890970799059033));
#31556=CARTESIAN_POINT('Ctrl Pts',(-1.58357141126859,1.42727158293121,1.48697727098601));
#31557=CARTESIAN_POINT('Ctrl Pts',(-1.54655823793102,0.84426039764207,1.76573546933512));
#31558=CARTESIAN_POINT('Ctrl Pts',(-1.50954506459346,0.261249212352931,
2.04449366768423));
#31559=CARTESIAN_POINT('Ctrl Pts',(-1.47253189125589,-0.473449431432427,
2.00600359245548));
#31560=CARTESIAN_POINT('Ctrl Pts',(-1.43551871791833,-1.02414158702801,
1.66785217850744));
#31561=CARTESIAN_POINT('Ctrl Pts',(-1.39850554458076,-1.57483374262357,
1.32970076455941));
#31562=CARTESIAN_POINT('Ctrl Pts',(-1.3614923712432,-1.94151941002937,0.691888011892126));
#31563=CARTESIAN_POINT('Ctrl Pts',(-1.32447919790564,-1.95665440631073,
0.0458389963489571));
#31564=CARTESIAN_POINT('Ctrl Pts',(-1.32360936264517,-1.95701008922699,
0.0306563961275103));
#31565=CARTESIAN_POINT('Ctrl Pts',(-1.3227395273847,-1.95717161681812,0.0154692471612372));
#31566=CARTESIAN_POINT('Ctrl Pts',(-1.32186969212423,-1.95714098413823,
0.000281429570410231));
#31567=CARTESIAN_POINT('Origin',(-9.8,0.,0.));
#31568=CARTESIAN_POINT('',(-0.520130307875779,-1.95245178959834,0.00157515171675247));
#31569=CARTESIAN_POINT('',(-0.62186969212423,-1.9522756157026,0.00152956335005719));
#31570=CARTESIAN_POINT('',(-9.8,-1.954,-2.39295984553393E-16));
#31571=CARTESIAN_POINT('Ctrl Pts',(-0.520130307875779,-1.95245178959834,
0.00157515171675247));
#31572=CARTESIAN_POINT('Ctrl Pts',(-0.531819405271675,-1.95405741327078,
0.20696418498022));
#31573=CARTESIAN_POINT('Ctrl Pts',(-0.543508502667571,-1.92424637327528,
0.41190437232312));
#31574=CARTESIAN_POINT('Ctrl Pts',(-0.555197600063466,-1.86107514875473,
0.605974135111533));
#31575=CARTESIAN_POINT('Ctrl Pts',(-0.59221077340103,-1.66104537708507,
1.22049016884649));
#31576=CARTESIAN_POINT('Ctrl Pts',(-0.629223946738595,-1.12652869134443,
1.72601355713792));
#31577=CARTESIAN_POINT('Ctrl Pts',(-0.66623712007616,-0.501894415972446,
1.89171586961104));
#31578=CARTESIAN_POINT('Ctrl Pts',(-0.703250293413725,0.122739859399543,
2.05741818208416));
#31579=CARTESIAN_POINT('Ctrl Pts',(-0.740263466751291,0.837491724402904,
1.88329941873898));
#31580=CARTESIAN_POINT('Ctrl Pts',(-0.777276640088856,1.31585516795866,
1.44883687645897));
#31581=CARTESIAN_POINT('Ctrl Pts',(-0.814289813426421,1.79421861151443,
1.01437433417895));
#31582=CARTESIAN_POINT('Ctrl Pts',(-0.851302986763983,2.03619363362259,
0.31956801296412));
#31583=CARTESIAN_POINT('Ctrl Pts',(-0.888316160101548,1.93117947666614,
-0.318073271893728));
#31584=CARTESIAN_POINT('Ctrl Pts',(-0.925329333439112,1.82616531970969,
-0.955714556751558));
#31585=CARTESIAN_POINT('Ctrl Pts',(-0.962342506776676,1.37416198368861,
-1.53619080525239));
#31586=CARTESIAN_POINT('Ctrl Pts',(-0.99935568011424,0.78171662343255,-1.79429636290242));
#31587=CARTESIAN_POINT('Ctrl Pts',(-1.0363688534518,0.189271263176508,-2.05240192055245));
#31588=CARTESIAN_POINT('Ctrl Pts',(-1.07338202678937,-0.543616121314529,
-1.98813678735172));
#31589=CARTESIAN_POINT('Ctrl Pts',(-1.11039520012693,-1.08208975290879,
-1.63085299191098));
#31590=CARTESIAN_POINT('Ctrl Pts',(-1.14697356937655,-1.61423778431377,
-1.27776630903335));
#31591=CARTESIAN_POINT('Ctrl Pts',(-1.18355193862616,-1.95651289934287,
-0.638504871936492));
#31592=CARTESIAN_POINT('Ctrl Pts',(-1.22013030787577,-1.95717923962325,
0.000142060037185308));
#31593=CARTESIAN_POINT('Ctrl Pts',(-1.32186969212423,-1.95714098413823,
0.000281429570410231));
#31594=CARTESIAN_POINT('Ctrl Pts',(-1.28572635404713,-1.95586813701901,
-0.630801777543932));
#31595=CARTESIAN_POINT('Ctrl Pts',(-1.24958301597004,-1.62281842013958,
-1.26303940726775));
#31596=CARTESIAN_POINT('Ctrl Pts',(-1.21343967789294,-1.10112109627574,
-1.61806369501833));
#31597=CARTESIAN_POINT('Ctrl Pts',(-1.17642650455538,-0.566868464802466,
-1.98163209242336));
#31598=CARTESIAN_POINT('Ctrl Pts',(-1.13941333121781,0.165221123300993,
-2.05448360881435));
#31599=CARTESIAN_POINT('Ctrl Pts',(-1.10240015788025,0.760646920128182,
-1.8033332830397));
#31600=CARTESIAN_POINT('Ctrl Pts',(-1.06538698454269,1.35607271695537,-1.55218295726506));
#31601=CARTESIAN_POINT('Ctrl Pts',(-1.02837381120512,1.81483472250629,-0.977030789324784));
#31602=CARTESIAN_POINT('Ctrl Pts',(-0.991360637867557,1.9273157180188,-0.3406682310869));
#31603=CARTESIAN_POINT('Ctrl Pts',(-0.954347464529993,2.03979671353132,
0.295694327150984));
#31604=CARTESIAN_POINT('Ctrl Pts',(-0.917334291192428,1.80599669900544,
0.993267275686475));
#31605=CARTESIAN_POINT('Ctrl Pts',(-0.880321117854863,1.33274677819716,
1.43331278513124));
#31606=CARTESIAN_POINT('Ctrl Pts',(-0.843307944517299,0.85949685738889,
1.87335829457599));
#31607=CARTESIAN_POINT('Ctrl Pts',(-0.806294771179734,0.146797030298244,
2.05587636493003));
#31608=CARTESIAN_POINT('Ctrl Pts',(-0.769281597842171,-0.479718878710562,
1.89748514905269));
#31609=CARTESIAN_POINT('Ctrl Pts',(-0.732268424504606,-1.10623478771939,
1.73909393317535));
#31610=CARTESIAN_POINT('Ctrl Pts',(-0.695255251167042,-1.64656677864637,
1.2397934310666));
#31611=CARTESIAN_POINT('Ctrl Pts',(-0.658242077829478,-1.85381294957979,
0.62769589808096));
#31612=CARTESIAN_POINT('Ctrl Pts',(-0.646117949261062,-1.92169902891681,
0.427195683774921));
#31613=CARTESIAN_POINT('Ctrl Pts',(-0.633993820692646,-1.95384592951114,
0.214592662906205));
#31614=CARTESIAN_POINT('Ctrl Pts',(-0.62186969212423,-1.9522756157026,0.00152956335005719));
#31615=CARTESIAN_POINT('Origin',(-20.9400562256037,0.,0.));
#31616=CARTESIAN_POINT('',(-0.29005622560372,-1.55426753261014,0.00125391427617921));
#31617=CARTESIAN_POINT('',(-0.151943774396314,-1.55328440515865,-0.00159394639174151));
#31618=CARTESIAN_POINT('',(-20.9400562256037,-1.5555,1.83293981223255E-13));
#31619=CARTESIAN_POINT('',(-3.11417115573063E-15,1.33818917000755,-0.797967911694413));
#31620=CARTESIAN_POINT('Ctrl Pts',(-0.29005622560372,-1.55426753261014,
0.00125391427617923));
#31621=CARTESIAN_POINT('Ctrl Pts',(-0.26473214966205,-1.55149841214987,
-0.352967927424292));
#31622=CARTESIAN_POINT('Ctrl Pts',(-0.202394900382818,-1.2557305975322,
-1.22904168662576));
#31623=CARTESIAN_POINT('Ctrl Pts',(-0.105709491848242,0.158347209672706,
-1.81077139712758));
#31624=CARTESIAN_POINT('Ctrl Pts',(-0.0343481592553409,1.09133363889359,
-1.20698403335016));
#31625=CARTESIAN_POINT('Ctrl Pts',(-3.13063377305189E-15,1.3381957767388,
-0.797970124357324));
#31626=CARTESIAN_POINT('',(0.,-0.31962117020207,-1.5223082991164));
#31627=CARTESIAN_POINT('Origin',(0.,0.,0.));
#31628=CARTESIAN_POINT('Ctrl Pts',(-0.151943774396314,-1.55328440515865,
-0.00159394639174141));
#31629=CARTESIAN_POINT('Ctrl Pts',(-0.138309022935107,-1.55435366600215,
-0.192572897595738));
#31630=CARTESIAN_POINT('Ctrl Pts',(-0.0876610981363355,-1.43339236355893,
-0.900161415364349));
#31631=CARTESIAN_POINT('Ctrl Pts',(-0.0370131733375646,-0.825376844998173,
-1.41612072810435));
#31632=CARTESIAN_POINT('Ctrl Pts',(0.,-0.319621170202026,-1.52230829911641));
#31633=CARTESIAN_POINT('Origin',(-20.9400562256037,0.,0.));
#31634=CARTESIAN_POINT('',(-0.990056225603717,-1.55803086347695,0.000113088223220368));
#31635=CARTESIAN_POINT('',(-0.851943774396308,-1.5541272877305,0.00121762323000714));
#31636=CARTESIAN_POINT('',(-20.9400562256037,-1.5555,1.83293981223255E-13));
#31637=CARTESIAN_POINT('Ctrl Pts',(-0.990056225603717,-1.55803086347695,
0.000113088223220355));
#31638=CARTESIAN_POINT('Ctrl Pts',(-0.953477856354101,-1.55750041705627,
-0.508287783161193));
#31639=CARTESIAN_POINT('Ctrl Pts',(-0.879886313766922,-1.00931895110904,
-1.53211702555747));
#31640=CARTESIAN_POINT('Ctrl Pts',(-0.769281597842172,0.734093027864279,
-1.68499263158297));
#31641=CARTESIAN_POINT('Ctrl Pts',(-0.658242077829484,1.81355749436498,
-0.29871196954151));
#31642=CARTESIAN_POINT('Ctrl Pts',(-0.547202557816791,1.23567804673567,
1.36060926789406));
#31643=CARTESIAN_POINT('Ctrl Pts',(-0.436163037804095,-0.47127670149265,
1.77643588465474));
#31644=CARTESIAN_POINT('Ctrl Pts',(-0.350447593733071,-1.4566697208266,
0.844492633449843));
#31645=CARTESIAN_POINT('Ctrl Pts',(-0.301745322999614,-1.55554570437189,
0.164755777756869));
#31646=CARTESIAN_POINT('Ctrl Pts',(-0.29005622560372,-1.55426753261014,
0.00125391427617923));
#31647=CARTESIAN_POINT('Ctrl Pts',(-0.851943774396308,-1.5541272877305,
0.00121762323000714));
#31648=CARTESIAN_POINT('Ctrl Pts',(-0.827054729627156,-1.55156109304348,
-0.346968447042236));
#31649=CARTESIAN_POINT('Ctrl Pts',(-0.765152511520438,-1.26385222212854,
-1.21679022327445));
#31650=CARTESIAN_POINT('Ctrl Pts',(-0.66623712007616,0.17630871353902,-1.82941001051451));
#31651=CARTESIAN_POINT('Ctrl Pts',(-0.555197600063458,1.63206374948406,
-0.84563791873513));
#31652=CARTESIAN_POINT('Ctrl Pts',(-0.444158080050773,1.59603445699364,
0.91144468152982));
#31653=CARTESIAN_POINT('Ctrl Pts',(-0.333118560038075,0.102187466450462,
1.83458816486299));
#31654=CARTESIAN_POINT('Ctrl Pts',(-0.235713791486592,-1.29129161789087,
1.17548693359841));
#31655=CARTESIAN_POINT('Ctrl Pts',(-0.175322196272671,-1.55145102879193,
0.325862443514162));
#31656=CARTESIAN_POINT('Ctrl Pts',(-0.151943774396314,-1.55328440515865,
-0.00159394639174141));
#31657=CARTESIAN_POINT('Origin',(-20.9400562256037,0.,0.));
#31658=CARTESIAN_POINT('',(-1.69005622560371,-1.5546041262458,-0.00134577896985914));
#31659=CARTESIAN_POINT('',(-1.55194377439631,-1.55800040983982,0.000224034645440537));
#31660=CARTESIAN_POINT('',(-20.9400562256037,-1.5555,1.83293981223255E-13));
#31661=CARTESIAN_POINT('Ctrl Pts',(-1.69005622560371,-1.5546041262458,-0.00134577896985951));
#31662=CARTESIAN_POINT('Ctrl Pts',(-1.67923673638372,-1.55585895440554,
-0.152585367351205));
#31663=CARTESIAN_POINT('Ctrl Pts',(-1.63140407382615,-1.46618838413473,
-0.819755125015001));
#31664=CARTESIAN_POINT('Ctrl Pts',(-1.54655823793103,-0.512809661837298,
-1.76498391861309));
#31665=CARTESIAN_POINT('Ctrl Pts',(-1.43551871791833,1.20351651524581,-1.3891323162764));
#31666=CARTESIAN_POINT('Ctrl Pts',(-1.32447919790564,1.82003619839053,0.256146657758448));
#31667=CARTESIAN_POINT('Ctrl Pts',(-1.21343967789295,0.77335431875082,1.66735307747278));
#31668=CARTESIAN_POINT('Ctrl Pts',(-1.10240015788025,-0.980037893435529,
1.55488263712548));
#31669=CARTESIAN_POINT('Ctrl Pts',(-1.02793900711718,-1.55527083732047,
0.526637965405178));
#31670=CARTESIAN_POINT('Ctrl Pts',(-0.990491029691664,-1.55803716885023,
0.00615640786072333));
#31671=CARTESIAN_POINT('Ctrl Pts',(-0.990056225603717,-1.55803086347695,
0.000113088223220355));
#31672=CARTESIAN_POINT('Ctrl Pts',(-1.55194377439631,-1.55800040983982,
0.000224034645440697));
#31673=CARTESIAN_POINT('Ctrl Pts',(-1.51580043631921,-1.55698714796992,
-0.502155662727371));
#31674=CARTESIAN_POINT('Ctrl Pts',(-1.44264392490454,-1.0203518296671,-1.52086555639993));
#31675=CARTESIAN_POINT('Ctrl Pts',(-1.33247424015232,0.714312595491066,
-1.69348504977325));
#31676=CARTESIAN_POINT('Ctrl Pts',(-1.22143472013962,1.8099179685225,-0.319919240308951));
#31677=CARTESIAN_POINT('Ctrl Pts',(-1.11039520012693,1.25156189493757,1.34600919589416));
#31678=CARTESIAN_POINT('Ctrl Pts',(-0.999355680114236,-0.45049222129505,
1.78189485367676));
#31679=CARTESIAN_POINT('Ctrl Pts',(-0.913205204870696,-1.45166145172168,
0.856751964042876));
#31680=CARTESIAN_POINT('Ctrl Pts',(-0.86406790296472,-1.55537735074439,
0.170828499053688));
#31681=CARTESIAN_POINT('Ctrl Pts',(-0.851943774396308,-1.5541272877305,
0.00121762323000714));
#31682=CARTESIAN_POINT('Origin',(-20.9400562256037,0.,0.));
#31683=CARTESIAN_POINT('',(-2.39005622560371,-1.55334130100463,0.000774134329562734));
#31684=CARTESIAN_POINT('',(-2.2519437743963,-1.55477365832743,-0.00137407056183869));
#31685=CARTESIAN_POINT('',(-20.9400562256037,-1.5555,1.83293981223255E-13));
#31686=CARTESIAN_POINT('Ctrl Pts',(-2.39005622560371,-1.55334130100463,
0.000774134329562682));
#31687=CARTESIAN_POINT('Ctrl Pts',(-2.36798244307577,-1.55194595900061,
-0.30841492839256));
#31688=CARTESIAN_POINT('Ctrl Pts',(-2.30889548721026,-1.31284241169292,
-1.1380386041486));
#31689=CARTESIAN_POINT('Ctrl Pts',(-2.21279535800718,0.0372963305200237,
-1.8375937199123));
#31690=CARTESIAN_POINT('Ctrl Pts',(-2.10175583799449,1.56324048867835,-0.966654456903947));
#31691=CARTESIAN_POINT('Ctrl Pts',(-1.9907163179818,1.66065158442465,0.787640790575088));
#31692=CARTESIAN_POINT('Ctrl Pts',(-1.87967679796911,0.2405125782874,1.82216778579164));
#31693=CARTESIAN_POINT('Ctrl Pts',(-1.77945676717641,-1.23962210290448,
1.25299318928825));
#31694=CARTESIAN_POINT('Ctrl Pts',(-1.71624990972128,-1.5515662219816,0.364801080977023));
#31695=CARTESIAN_POINT('Ctrl Pts',(-1.69005622560371,-1.5546041262458,-0.00134577896985951));
#31696=CARTESIAN_POINT('Ctrl Pts',(-2.2519437743963,-1.55477365832743,-0.00137407056183876));
#31697=CARTESIAN_POINT('Ctrl Pts',(-2.24155931634882,-1.55601358341305,
-0.146492457084467));
#31698=CARTESIAN_POINT('Ctrl Pts',(-2.19416168496378,-1.4708593613734,-0.807427026857451));
#31699=CARTESIAN_POINT('Ctrl Pts',(-2.10975088024117,-0.533449971191177,
-1.75885550507193));
#31700=CARTESIAN_POINT('Ctrl Pts',(-1.99871136022847,1.18716147401266,-1.40313541149553));
#31701=CARTESIAN_POINT('Ctrl Pts',(-1.88767184021578,1.82291149503699,0.234809115073605));
#31702=CARTESIAN_POINT('Ctrl Pts',(-1.77663232020309,0.792833618333258,
1.65817871653077));
#31703=CARTESIAN_POINT('Ctrl Pts',(-1.66559280019039,-0.96175759007224,
1.56625756194791));
#31704=CARTESIAN_POINT('Ctrl Pts',(-1.5906966182548,-1.5524246457012,0.538851764154201));
#31705=CARTESIAN_POINT('Ctrl Pts',(-1.55281360965677,-1.55802479527153,
0.0123144390786119));
#31706=CARTESIAN_POINT('Ctrl Pts',(-1.55194377439631,-1.55800040983982,
0.000224034645440697));
#31707=CARTESIAN_POINT('Origin',(-20.9400562256037,0.,0.));
#31708=CARTESIAN_POINT('',(-3.09005622560371,-1.55741714054868,0.000874486562257179));
#31709=CARTESIAN_POINT('',(-2.9519437743963,-1.5532548564925,0.00068838530571283));
#31710=CARTESIAN_POINT('',(-20.9400562256037,-1.5555,1.83293981223255E-13));
#31711=CARTESIAN_POINT('Ctrl Pts',(-3.09005622560371,-1.55741714054868,
0.000874486562257217));
#31712=CARTESIAN_POINT('Ctrl Pts',(-3.05672814976782,-1.55429140820636,
-0.462834767864285));
#31713=CARTESIAN_POINT('Ctrl Pts',(-2.98638690059437,-1.08874094224246,
-1.44697424618156));
#31714=CARTESIAN_POINT('Ctrl Pts',(-2.87903247808334,0.584003181164767,
-1.74272257439688));
#31715=CARTESIAN_POINT('Ctrl Pts',(-2.76799295807065,1.78048817758317,-0.456074046366774));
#31716=CARTESIAN_POINT('Ctrl Pts',(-2.65695343805795,1.34991305530291,1.24734775817125));
#31717=CARTESIAN_POINT('Ctrl Pts',(-2.54591391804527,-0.314250542958959,
1.81090813803855));
#31718=CARTESIAN_POINT('Ctrl Pts',(-2.45694818056051,-1.41750787088368,
0.93655130592161));
#31719=CARTESIAN_POINT('Ctrl Pts',(-2.40499561641333,-1.55428565929415,
0.210031258078886));
#31720=CARTESIAN_POINT('Ctrl Pts',(-2.39005622560371,-1.55334130100463,
0.000774134329562682));
#31721=CARTESIAN_POINT('Ctrl Pts',(-2.9519437743963,-1.5532548564925,0.000688385305712795));
#31722=CARTESIAN_POINT('Ctrl Pts',(-2.93030502304087,-1.55204250277955,
-0.302449348443936));
#31723=CARTESIAN_POINT('Ctrl Pts',(-2.87165309834789,-1.32000917179155,
-1.12581972118214));
#31724=CARTESIAN_POINT('Ctrl Pts',(-2.77598800031732,0.0157677844803547,
-1.83790448190824));
#31725=CARTESIAN_POINT('Ctrl Pts',(-2.66494848030463,1.55180958399743,-0.984900257957451));
#31726=CARTESIAN_POINT('Ctrl Pts',(-2.55390896029194,1.66976418974896,0.768133489551486));
#31727=CARTESIAN_POINT('Ctrl Pts',(-2.44286944027925,0.261841363970268,
1.81922527888795));
#31728=CARTESIAN_POINT('Ctrl Pts',(-2.34221437831403,-1.23131260497695,
1.26503319844093));
#31729=CARTESIAN_POINT('Ctrl Pts',(-2.27857248968638,-1.55159413639811,
0.370750905089191));
#31730=CARTESIAN_POINT('Ctrl Pts',(-2.2519437743963,-1.55477365832743,-0.00137407056183876));
#31731=CARTESIAN_POINT('Origin',(-20.9400562256037,0.,0.));
#31732=CARTESIAN_POINT('',(-3.79005622560371,-1.55594287263106,-0.00137858150463178));
#31733=CARTESIAN_POINT('',(-3.6519437743963,-1.55727935086102,0.000957570549856082));
#31734=CARTESIAN_POINT('',(-20.9400562256037,-1.5555,1.83293981223255E-13));
#31735=CARTESIAN_POINT('Ctrl Pts',(-3.79005622560371,-1.55594287263106,
-0.00137858150463233));
#31736=CARTESIAN_POINT('Ctrl Pts',(-3.78248702979744,-1.55691314113539,
-0.106951986014344));
#31737=CARTESIAN_POINT('Ctrl Pts',(-3.7379046606536,-1.49901533715616,-0.727718784499475));
#31738=CARTESIAN_POINT('Ctrl Pts',(-3.6563091181722,-0.665127613333747,
-1.71340215497423));
#31739=CARTESIAN_POINT('Ctrl Pts',(-3.5452695981595,1.07748310522118,-1.48901707332687));
#31740=CARTESIAN_POINT('Ctrl Pts',(-3.43423007814681,1.83545949062223,0.0960736434662692));
#31741=CARTESIAN_POINT('Ctrl Pts',(-3.32319055813411,0.916141426756487,
1.59336956568948));
#31742=CARTESIAN_POINT('Ctrl Pts',(-3.21215103812143,-0.840372411640004,
1.63459961350804));
#31743=CARTESIAN_POINT('Ctrl Pts',(-3.13443959394462,-1.53221855341299,
0.618052683999356));
#31744=CARTESIAN_POINT('Ctrl Pts',(-3.09374132310538,-1.55776275391389,
0.0521469879633103));
#31745=CARTESIAN_POINT('Ctrl Pts',(-3.09005622560371,-1.55741714054868,
0.000874486562257217));
#31746=CARTESIAN_POINT('Ctrl Pts',(-3.6519437743963,-1.55727935086102,0.000957570549856073));
#31747=CARTESIAN_POINT('Ctrl Pts',(-3.61905072973292,-1.55396652622214,
-0.456805336982523));
#31748=CARTESIAN_POINT('Ctrl Pts',(-3.54914451173199,-1.09885245176768,
-1.43539894970098));
#31749=CARTESIAN_POINT('Ctrl Pts',(-3.44222512039348,0.563548452575144,
-1.74944409679311));
#31750=CARTESIAN_POINT('Ctrl Pts',(-3.3311856003808,1.77502341045502,-0.476899778205122));
#31751=CARTESIAN_POINT('Ctrl Pts',(-3.22014608036809,1.36443210709099,1.23144895602193));
#31752=CARTESIAN_POINT('Ctrl Pts',(-3.10910656035541,-0.293015589158281,
1.81446503711471));
#31753=CARTESIAN_POINT('Ctrl Pts',(-3.01970579169814,-1.41188410329576,
0.948880020508335));
#31754=CARTESIAN_POINT('Ctrl Pts',(-2.96731819637844,-1.55411623880003,
0.21606899395653));
#31755=CARTESIAN_POINT('Ctrl Pts',(-2.9519437743963,-1.5532548564925,0.000688385305712795));
#31756=CARTESIAN_POINT('Origin',(-20.9400562256037,0.,0.));
#31757=CARTESIAN_POINT('',(-4.4900562256037,-1.55296096245849,7.2602473186181E-5));
#31758=CARTESIAN_POINT('',(-4.3519437743963,-1.55612556903524,-0.00135081906484813));
#31759=CARTESIAN_POINT('',(-20.9400562256037,-1.5555,1.83293981223255E-13));
#31760=CARTESIAN_POINT('Ctrl Pts',(-4.4900562256037,-1.55296096245849,7.26024731861723E-5));
#31761=CARTESIAN_POINT('Ctrl Pts',(-4.47123273648949,-1.55285093046517,
-0.263750775239748));
#31762=CARTESIAN_POINT('Ctrl Pts',(-4.4153960740377,-1.36387406460508,-1.04648565772416));
#31763=CARTESIAN_POINT('Ctrl Pts',(-4.32254623824836,-0.123474165349735,
-1.83382000675687));
#31764=CARTESIAN_POINT('Ctrl Pts',(-4.21150671823566,1.4727595977204,-1.09960031557524));
#31765=CARTESIAN_POINT('Ctrl Pts',(-4.10046719822297,1.72314426360711,0.639465036955492));
#31766=CARTESIAN_POINT('Ctrl Pts',(-3.98942767821027,0.398871290133161,
1.79416927311721));
#31767=CARTESIAN_POINT('Ctrl Pts',(-3.88595735400385,-1.17478343605878,
1.34236238614872));
#31768=CARTESIAN_POINT('Ctrl Pts',(-3.819500203135,-1.55216855303728,0.409299254007138));
#31769=CARTESIAN_POINT('Ctrl Pts',(-3.79005622560371,-1.55594287263106,
-0.00137858150463233));
#31770=CARTESIAN_POINT('Ctrl Pts',(-4.3519437743963,-1.55612556903524,-0.00135081906484836));
#31771=CARTESIAN_POINT('Ctrl Pts',(-4.34480960976254,-1.55703324266528,
-0.100826422108305));
#31772=CARTESIAN_POINT('Ctrl Pts',(-4.30066227179122,-1.50305305182904,
-0.715415977812441));
#31773=CARTESIAN_POINT('Ctrl Pts',(-4.21950176048233,-0.685153134847353,
-1.70549309232754));
#31774=CARTESIAN_POINT('Ctrl Pts',(-4.10846224046965,1.0599664669302,-1.50153674452297));
#31775=CARTESIAN_POINT('Ctrl Pts',(-3.99742272045695,1.83645893175252,0.0745660657000111));
#31776=CARTESIAN_POINT('Ctrl Pts',(-3.88638320044426,0.93474362991831,1.5825283101715));
#31777=CARTESIAN_POINT('Ctrl Pts',(-3.77534368043157,-0.821166662308707,
1.64433172410147));
#31778=CARTESIAN_POINT('Ctrl Pts',(-3.69719720508225,-1.52881274645944,
0.630314108528291));
#31779=CARTESIAN_POINT('Ctrl Pts',(-3.65606390307049,-1.55769430982656,
0.0582961994486606));
#31780=CARTESIAN_POINT('Ctrl Pts',(-3.6519437743963,-1.55727935086102,0.000957570549856073));
#31781=CARTESIAN_POINT('Origin',(-20.9400562256037,0.,0.));
#31782=CARTESIAN_POINT('',(-5.1900562256037,-1.55620847966863,0.00133559623655165));
#31783=CARTESIAN_POINT('',(-5.05194377439629,-1.55295797459783,-2.70762857591493E-5));
#31784=CARTESIAN_POINT('',(-20.9400562256037,-1.5555,1.83293981223255E-13));
#31785=CARTESIAN_POINT('Ctrl Pts',(-5.1900562256037,-1.55620847966863,0.00133559623655161));
#31786=CARTESIAN_POINT('Ctrl Pts',(-5.15997844318154,-1.5524016656663,-0.417997969474535));
#31787=CARTESIAN_POINT('Ctrl Pts',(-5.0928874874218,-1.16138848763123,-1.35961338929137));
#31788=CARTESIAN_POINT('Ctrl Pts',(-4.98878335832452,0.429432903867215,
-1.78710074359752));
#31789=CARTESIAN_POINT('Ctrl Pts',(-4.87774383831181,1.73380656428109,-0.6099643303886));
#31790=CARTESIAN_POINT('Ctrl Pts',(-4.76670431829913,1.45377907542383,1.12457462471391));
#31791=CARTESIAN_POINT('Ctrl Pts',(-4.65566479828643,-0.154752576089497,
1.83144569312997));
#31792=CARTESIAN_POINT('Ctrl Pts',(-4.56344876738796,-1.37316082212235,
1.02857522543411));
#31793=CARTESIAN_POINT('Ctrl Pts',(-4.50824590982705,-1.5530672895693,0.255012794603092));
#31794=CARTESIAN_POINT('Ctrl Pts',(-4.4900562256037,-1.55296096245849,7.26024731861723E-5));
#31795=CARTESIAN_POINT('Ctrl Pts',(-5.05194377439629,-1.55295826129353,
-2.70732320311814E-5));
#31796=CARTESIAN_POINT('Ctrl Pts',(-5.03355531645459,-1.55299833977778,
-0.257754302019052));
#31797=CARTESIAN_POINT('Ctrl Pts',(-4.97815368517533,-1.37027115613983,
-1.03419383952361));
#31798=CARTESIAN_POINT('Ctrl Pts',(-4.8857388805585,-0.144947467941284,
-1.83224772825777));
#31799=CARTESIAN_POINT('Ctrl Pts',(-4.7746993605458,1.45977754246094,-1.11677707385809));
#31800=CARTESIAN_POINT('Ctrl Pts',(-4.66365984053311,1.73051682250325,0.619235846185912));
#31801=CARTESIAN_POINT('Ctrl Pts',(-4.55262032052042,0.419861211735448,
1.78937365271996));
#31802=CARTESIAN_POINT('Ctrl Pts',(-4.44871496514148,-1.16561614495599,
1.35420997741823));
#31803=CARTESIAN_POINT('Ctrl Pts',(-4.38182278310011,-1.55232408845772,
0.415268723900115));
#31804=CARTESIAN_POINT('Ctrl Pts',(-4.3519437743963,-1.55612556903524,-0.00135081906484836));
#31805=CARTESIAN_POINT('Origin',(-20.9400562256037,0.,0.));
#31806=CARTESIAN_POINT('',(-5.8900562256037,-1.55721324091966,-0.000993547179071312));
#31807=CARTESIAN_POINT('',(-5.75194377439629,-1.55602652096245,0.00136684493791416));
#31808=CARTESIAN_POINT('',(-20.9400562256037,-1.5555,1.83293981223255E-13));
#31809=CARTESIAN_POINT('Ctrl Pts',(-5.8900562256037,-1.55721324091966,-0.000993547179071299));
#31810=CARTESIAN_POINT('Ctrl Pts',(-5.88573732321115,-1.55766070941293,
-0.061105153849158));
#31811=CARTESIAN_POINT('Ctrl Pts',(-5.84440524748104,-1.52723085673784,
-0.635918540321862));
#31812=CARTESIAN_POINT('Ctrl Pts',(-5.76605999841336,-0.812353568509229,
-1.64870354109554));
#31813=CARTESIAN_POINT('Ctrl Pts',(-5.65502047840067,0.943200812016622,
-1.57750242944403));
#31814=CARTESIAN_POINT('Ctrl Pts',(-5.54398095838797,1.83683179154747,-0.0647352782582765));
#31815=CARTESIAN_POINT('Ctrl Pts',(-5.43294143837528,1.05191427466497,1.50718878892018));
#31816=CARTESIAN_POINT('Ctrl Pts',(-5.32190191836259,-0.694272059656186,
1.70180139671801));
#31817=CARTESIAN_POINT('Ctrl Pts',(-5.24094018077207,-1.50487070765057,
0.709796123886388));
#31818=CARTESIAN_POINT('Ctrl Pts',(-5.1969916165191,-1.55708626190928,0.0980263083819725));
#31819=CARTESIAN_POINT('Ctrl Pts',(-5.1900562256037,-1.55620847966863,0.00133559623655161));
#31820=CARTESIAN_POINT('Ctrl Pts',(-5.75194377439629,-1.55602652096245,
0.00136684493791428));
#31821=CARTESIAN_POINT('Ctrl Pts',(-5.72230102314664,-1.55223721629162,
-0.412026212646332));
#31822=CARTESIAN_POINT('Ctrl Pts',(-5.65564509855944,-1.17060922994658,
-1.34777943804002));
#31823=CARTESIAN_POINT('Ctrl Pts',(-5.55197600063464,0.408468929309301,
-1.79200854907483));
#31824=CARTESIAN_POINT('Ctrl Pts',(-5.44093648062197,1.726542296104,-0.630232660159929));
#31825=CARTESIAN_POINT('Ctrl Pts',(-5.32989696060926,1.46685280597546,1.1074675398269));
#31826=CARTESIAN_POINT('Ctrl Pts',(-5.21885744059658,-0.133287989090187,
1.83313278791599));
#31827=CARTESIAN_POINT('Ctrl Pts',(-5.12620637852558,-1.36680944890504,
1.04087016911624));
#31828=CARTESIAN_POINT('Ctrl Pts',(-5.07056848979215,-1.55291766787536,
0.261011470681804));
#31829=CARTESIAN_POINT('Ctrl Pts',(-5.05194377439629,-1.55295826129353,
-2.70732320311814E-5));
#31830=CARTESIAN_POINT('Origin',(-20.9400562256037,0.,0.));
#31831=CARTESIAN_POINT('',(-6.5900562256037,-1.55321890847038,-0.000648066932651872));
#31832=CARTESIAN_POINT('',(-6.45194377439629,-1.55735540394282,-0.000913172825708491));
#31833=CARTESIAN_POINT('',(-20.9400562256037,-1.5555,1.83293981223255E-13));
#31834=CARTESIAN_POINT('Ctrl Pts',(-6.5900562256037,-1.55321890847038,-0.000648066932651941));
#31835=CARTESIAN_POINT('Ctrl Pts',(-6.5744830299032,-1.55403921561424,-0.218825949717235));
#31836=CARTESIAN_POINT('Ctrl Pts',(-6.52189666086514,-1.40928295541454,
-0.954512421279383));
#31837=CARTESIAN_POINT('Ctrl Pts',(-6.43229711848952,-0.283299401454877,
-1.81600747130234));
#31838=CARTESIAN_POINT('Ctrl Pts',(-6.32125759847683,1.37100397883372,-1.22412817005115));
#31839=CARTESIAN_POINT('Ctrl Pts',(-6.21021807846413,1.77244540527444,0.486393844545889));
#31840=CARTESIAN_POINT('Ctrl Pts',(-6.09917855845144,0.55417642399643,1.75243549889208));
#31841=CARTESIAN_POINT('Ctrl Pts',(-5.9924579408313,-1.10343237309906,1.43009714852447));
#31842=CARTESIAN_POINT('Ctrl Pts',(-5.92275049654872,-1.5538258857936,0.454053818281797));
#31843=CARTESIAN_POINT('Ctrl Pts',(-5.8900562256037,-1.55721324091966,-0.000993547179071299));
#31844=CARTESIAN_POINT('Ctrl Pts',(-6.45194377439629,-1.55735540394282,
-0.000913172825708474));
#31845=CARTESIAN_POINT('Ctrl Pts',(-6.44805990317626,-1.55773235374386,
-0.0549569394560008));
#31846=CARTESIAN_POINT('Ctrl Pts',(-6.40716285861867,-1.53067193784369,
-0.623654417057565));
#31847=CARTESIAN_POINT('Ctrl Pts',(-6.3292526407235,-0.831611090304988,
-1.6390742816145));
#31848=CARTESIAN_POINT('Ctrl Pts',(-6.21821312071081,0.924656853680087,
-1.58844301412132));
#31849=CARTESIAN_POINT('Ctrl Pts',(-6.10717360069812,1.83594738678564,-0.0862478934429835));
#31850=CARTESIAN_POINT('Ctrl Pts',(-5.99613408068542,1.06949761739632,1.49476297537502));
#31851=CARTESIAN_POINT('Ctrl Pts',(-5.88509456067274,-0.674289122018889,
1.70981744232983));
#31852=CARTESIAN_POINT('Ctrl Pts',(-5.80369779190968,-1.50087042795734,
0.722096848042709));
#31853=CARTESIAN_POINT('Ctrl Pts',(-5.7593141964842,-1.55696869986509,0.104153569994228));
#31854=CARTESIAN_POINT('Ctrl Pts',(-5.75194377439629,-1.55602652096245,
0.00136684493791428));
#31855=CARTESIAN_POINT('Origin',(-20.9400562256037,0.,0.));
#31856=CARTESIAN_POINT('',(-7.29005622560369,-1.55485270523888,0.00138463193874137));
#31857=CARTESIAN_POINT('',(-7.15194377439629,-1.55330049259386,-0.00073539602550049));
#31858=CARTESIAN_POINT('',(-20.9400562256037,-1.5555,1.83293981223255E-13));
#31859=CARTESIAN_POINT('Ctrl Pts',(-7.29005622560369,-1.55485270523888,
0.00138463193874141));
#31860=CARTESIAN_POINT('Ctrl Pts',(-7.26322873659525,-1.55161198643692,
-0.373469770863784));
#31861=CARTESIAN_POINT('Ctrl Pts',(-7.19938807424924,-1.22747835831958,
-1.27052714563407));
#31862=CARTESIAN_POINT('Ctrl Pts',(-7.09853423856569,0.271575099355961,
-1.81779774785327));
#31863=CARTESIAN_POINT('Ctrl Pts',(-6.98749471855298,1.67385177993814,-0.75918502717621));
#31864=CARTESIAN_POINT('Ctrl Pts',(-6.8764551985403,1.54651567759537,0.993192300434498));
#31865=CARTESIAN_POINT('Ctrl Pts',(-6.7654156785276,0.00593010012215213,
1.83796260043647));
#31866=CARTESIAN_POINT('Ctrl Pts',(-6.6699493542154,-1.32324876481184,1.12023263145137));
#31867=CARTESIAN_POINT('Ctrl Pts',(-6.61149620324077,-1.55208957270924,
0.299722455455113));
#31868=CARTESIAN_POINT('Ctrl Pts',(-6.5900562256037,-1.55321890847038,-0.000648066932651941));
#31869=CARTESIAN_POINT('Ctrl Pts',(-7.15194377439629,-1.55330049259386,
-0.000735396025500611));
#31870=CARTESIAN_POINT('Ctrl Pts',(-7.13680560986831,-1.55420812252312,
-0.212790680832262));
#31871=CARTESIAN_POINT('Ctrl Pts',(-7.08465427200277,-1.41494999776031,
-0.942184803894316));
#31872=CARTESIAN_POINT('Ctrl Pts',(-6.99548976079967,-0.304553073520857,
-1.8125641868848));
#31873=CARTESIAN_POINT('Ctrl Pts',(-6.88445024078697,1.35657016098623,-1.24010439257756));
#31874=CARTESIAN_POINT('Ctrl Pts',(-6.77341072077428,1.77802146990873,0.465597636067849));
#31875=CARTESIAN_POINT('Ctrl Pts',(-6.66237120076158,0.574666806591611,
1.74582346403357));
#31876=CARTESIAN_POINT('Ctrl Pts',(-6.55521555196892,-1.09337608577705,
1.44169011708872));
#31877=CARTESIAN_POINT('Ctrl Pts',(-6.48507307651382,-1.55414003372731,
0.460078495237449));
#31878=CARTESIAN_POINT('Ctrl Pts',(-6.45194377439629,-1.55735540394282,
-0.000913172825708474));
#31879=CARTESIAN_POINT('Origin',(-20.9400562256037,0.,0.));
#31880=CARTESIAN_POINT('',(-7.9900562256037,-1.5579805623394,-0.000274378025309067));
#31881=CARTESIAN_POINT('',(-7.85194377439629,-1.55468095905983,0.00135958930439439));
#31882=CARTESIAN_POINT('',(-20.9400562256037,-1.5555,1.83293981223255E-13));
#31883=CARTESIAN_POINT('Ctrl Pts',(-7.9900562256037,-1.5579805623394,-0.000274378025309032));
#31884=CARTESIAN_POINT('Ctrl Pts',(-7.98898761662487,-1.55801680100739,
-0.015128171441536));
#31885=CARTESIAN_POINT('Ctrl Pts',(-7.95090583430849,-1.55110026292883,
-0.544434940735035));
#31886=CARTESIAN_POINT('Ctrl Pts',(-7.87581087865453,-0.953360544007956,
-1.57138326318549));
#31887=CARTESIAN_POINT('Ctrl Pts',(-7.76477135864184,0.80169783694629,-1.65391120224947));
#31888=CARTESIAN_POINT('Ctrl Pts',(-7.65373183862914,1.82414221101299,-0.225048618505586));
#31889=CARTESIAN_POINT('Ctrl Pts',(-7.54269231861645,1.17963418386913,1.40946971550936));
#31890=CARTESIAN_POINT('Ctrl Pts',(-7.43165279860376,-0.54285670200082,
1.75597502481768));
#31891=CARTESIAN_POINT('Ctrl Pts',(-7.34744076759951,-1.47296469184551,
0.801794893149571));
#31892=CARTESIAN_POINT('Ctrl Pts',(-7.30024190993282,-1.55608312000881,
0.143706882639392));
#31893=CARTESIAN_POINT('Ctrl Pts',(-7.29005622560369,-1.55485270523888,
0.00138463193874141));
#31894=CARTESIAN_POINT('Ctrl Pts',(-7.85194377439629,-1.55468095905983,
0.0013595893043942));
#31895=CARTESIAN_POINT('Ctrl Pts',(-7.82555131656036,-1.55157709491204,
-0.367519572225172));
#31896=CARTESIAN_POINT('Ctrl Pts',(-7.76214568538688,-1.23583930007717,
-1.2584972052081));
#31897=CARTESIAN_POINT('Ctrl Pts',(-7.66172688087582,0.250262368674325,
-1.82085426462248));
#31898=CARTESIAN_POINT('Ctrl Pts',(-7.55068736086313,1.66484362245829,-0.778740790589749));
#31899=CARTESIAN_POINT('Ctrl Pts',(-7.43964784085044,1.55804400070415,0.97500789639785));
#31900=CARTESIAN_POINT('Ctrl Pts',(-7.32860832083774,0.0274599982776329,
1.83776697507137));
#31901=CARTESIAN_POINT('Ctrl Pts',(-7.23270696535303,-1.3161301222519,1.13245711826584));
#31902=CARTESIAN_POINT('Ctrl Pts',(-7.17381878320588,-1.55198894569782,
0.305689548339082));
#31903=CARTESIAN_POINT('Ctrl Pts',(-7.15194377439629,-1.55330049259386,
-0.000735396025500611));
#31904=CARTESIAN_POINT('Origin',(-20.9400562256037,0.,0.));
#31905=CARTESIAN_POINT('',(-8.69005622560369,-1.55406204600757,-0.00119630707125469));
#31906=CARTESIAN_POINT('',(-8.55194377439629,-1.55801888457014,-0.000163493340269438));
#31907=CARTESIAN_POINT('',(-20.9400562256037,-1.5555,1.83293981223255E-13));
#31908=CARTESIAN_POINT('Ctrl Pts',(-8.6900562256037,-1.55406204600757,-0.00119630707125503));
#31909=CARTESIAN_POINT('Ctrl Pts',(-8.67773332331692,-1.55530151980103,
-0.173603109199959));
#31910=CARTESIAN_POINT('Ctrl Pts',(-8.62839724769259,-1.44936656402823,
-0.862372755859578));
#31911=CARTESIAN_POINT('Ctrl Pts',(-8.5420479987307,-0.44095583657419,-1.78429247515137));
#31912=CARTESIAN_POINT('Ctrl Pts',(-8.43100847871798,1.25875262728536,-1.33928470087313));
#31913=CARTESIAN_POINT('Ctrl Pts',(-8.31996895870532,1.8081775760136,0.329599059907972));
#31914=CARTESIAN_POINT('Ctrl Pts',(-8.2089294386926,0.705239055515858,1.69728593974785));
#31915=CARTESIAN_POINT('Ctrl Pts',(-8.09895852765874,-1.02535025064066,
1.51570965553032));
#31916=CARTESIAN_POINT('Ctrl Pts',(-8.02600078996244,-1.55676161026297,
0.499359392606125));
#31917=CARTESIAN_POINT('Ctrl Pts',(-7.9900562256037,-1.5579805623394,-0.000274378025309032));
#31918=CARTESIAN_POINT('Ctrl Pts',(-8.55194377439629,-1.55801888457014,
-0.0001634933402693));
#31919=CARTESIAN_POINT('Ctrl Pts',(-8.55131019658998,-1.55803205717942,
-0.00896971795875712));
#31920=CARTESIAN_POINT('Ctrl Pts',(-8.51366344544611,-1.5539786003993,-0.532216984914002));
#31921=CARTESIAN_POINT('Ctrl Pts',(-8.43900352096468,-0.971702639962959,
-1.56010752374873));
#31922=CARTESIAN_POINT('Ctrl Pts',(-8.32796400095197,0.782268521994644,
-1.66318894466765));
#31923=CARTESIAN_POINT('Ctrl Pts',(-8.2169244809393,1.82138073092891,-0.246401581101293));
#31924=CARTESIAN_POINT('Ctrl Pts',(-8.10588496092658,1.1960640567365,1.39555446986186));
#31925=CARTESIAN_POINT('Ctrl Pts',(-7.99484544091391,-0.522249555601089,
1.76221363853615));
#31926=CARTESIAN_POINT('Ctrl Pts',(-7.91019837873713,-1.46833344136842,
0.814121917015574));
#31927=CARTESIAN_POINT('Ctrl Pts',(-7.86256448989793,-1.55592999991363,
0.149802021359961));
#31928=CARTESIAN_POINT('Ctrl Pts',(-7.85194377439629,-1.55468095905983,
0.0013595893043942));
#31929=CARTESIAN_POINT('Origin',(-20.9400562256037,0.,0.));
#31930=CARTESIAN_POINT('',(-9.3900562256037,-1.55371612834885,0.00103887111830012));
#31931=CARTESIAN_POINT('',(-9.25194377439629,-1.55421089288766,-0.00124746091003075));
#31932=CARTESIAN_POINT('',(-20.9400562256037,-1.5555,1.83293981223255E-13));
#31933=CARTESIAN_POINT('Ctrl Pts',(-9.3900562256037,-1.55371612834885,0.00103887111830016));
#31934=CARTESIAN_POINT('Ctrl Pts',(-9.36647903000898,-1.55168635657405,
-0.329008869350852));
#31935=CARTESIAN_POINT('Ctrl Pts',(-9.3058886610767,-1.28725468228538,-1.18016031646684));
#31936=CARTESIAN_POINT('Ctrl Pts',(-9.20828511880685,0.111638249353674,
-1.83457858593517));
#31937=CARTESIAN_POINT('Ctrl Pts',(-9.09724559879415,1.60108280900731,-0.902593776508504));
#31938=CARTESIAN_POINT('Ctrl Pts',(-8.98620607878146,1.62741291579734,0.854206584022058));
#31939=CARTESIAN_POINT('Ctrl Pts',(-8.87516655876877,0.166567378401736,
1.83040896936805));
#31940=CARTESIAN_POINT('Ctrl Pts',(-8.77644994104285,-1.26747859705886,
1.21122555034046));
#31941=CARTESIAN_POINT('Ctrl Pts',(-8.71474649665449,-1.55157862585143,
0.344239417119107));
#31942=CARTESIAN_POINT('Ctrl Pts',(-8.6900562256037,-1.55406204600757,-0.00119630707125503));
#31943=CARTESIAN_POINT('Ctrl Pts',(-9.25194377439629,-1.55421089288766,
-0.00124746091003079));
#31944=CARTESIAN_POINT('Ctrl Pts',(-9.24005590328203,-1.55546589319888,
-0.167527666085323));
#31945=CARTESIAN_POINT('Ctrl Pts',(-9.19115485883021,-1.4543434475797,-0.850039222709116));
#31946=CARTESIAN_POINT('Ctrl Pts',(-9.10524064104083,-0.461827170446667,
-1.77900454490864));
#31947=CARTESIAN_POINT('Ctrl Pts',(-8.99420112102814,1.24297754506556,-1.35393808153518));
#31948=CARTESIAN_POINT('Ctrl Pts',(-8.88316160101544,1.81191445877564,0.308395039272923));
#31949=CARTESIAN_POINT('Ctrl Pts',(-8.77212208100275,0.725073034805075,
1.68890810891739));
#31950=CARTESIAN_POINT('Ctrl Pts',(-8.66171613879637,-1.01437844712226,
1.5269787503532));
#31951=CARTESIAN_POINT('Ctrl Pts',(-8.58832336992754,-1.55726252253713,
0.505483779320834));
#31952=CARTESIAN_POINT('Ctrl Pts',(-8.55194377439629,-1.55801888457014,
-0.0001634933402693));
#31953=CARTESIAN_POINT('Origin',(-20.9400562256037,0.,0.));
#31954=CARTESIAN_POINT('',(-10.0900562256037,-1.55780423998256,0.000547110510323483));
#31955=CARTESIAN_POINT('',(-9.95194377439629,-1.5535960288726,0.000967876971002882));
#31956=CARTESIAN_POINT('',(-20.9400562256037,-1.5555,1.83293981223255E-13));
#31957=CARTESIAN_POINT('Ctrl Pts',(-10.0900562256037,-1.55780423998256,
0.000547110510323474));
#31958=CARTESIAN_POINT('Ctrl Pts',(-10.055224736701,-1.55559939196281,-0.483761196717675));
#31959=CARTESIAN_POINT('Ctrl Pts',(-9.98338007446081,-1.05285972037605,
-1.48666276859663));
#31960=CARTESIAN_POINT('Ctrl Pts',(-9.874522238883,0.654057457242615,-1.71765844372971));
#31961=CARTESIAN_POINT('Ctrl Pts',(-9.76348271887031,1.79748789421279,-0.38363909713309));
#31962=CARTESIAN_POINT('Ctrl Pts',(-9.65244319885762,1.29832339351032,1.30096043466144));
#31963=CARTESIAN_POINT('Ctrl Pts',(-9.54140367884492,-0.387285500229918,
1.79670577112734));
#31964=CARTESIAN_POINT('Ctrl Pts',(-9.45394135442695,-1.43622080995592,
0.893931513220443));
#31965=CARTESIAN_POINT('Ctrl Pts',(-9.40349220334654,-1.55487283794477,
0.18912375497161));
#31966=CARTESIAN_POINT('Ctrl Pts',(-9.3900562256037,-1.55371612834885,0.00103887111830016));
#31967=CARTESIAN_POINT('Ctrl Pts',(-9.95194377439629,-1.5535960288726,0.000967876971002899));
#31968=CARTESIAN_POINT('Ctrl Pts',(-9.92880160997409,-1.55174879348202,
-0.323052877225753));
#31969=CARTESIAN_POINT('Ctrl Pts',(-9.86864627221432,-1.29479054227638,
-1.16798978252056));
#31970=CARTESIAN_POINT('Ctrl Pts',(-9.77147776111699,0.0901399223399556,
-1.83576041480606));
#31971=CARTESIAN_POINT('Ctrl Pts',(-9.66043824110429,1.59039972425115,-0.921287264250532));
#31972=CARTESIAN_POINT('Ctrl Pts',(-9.54939872109161,1.63730757628732,0.835084071696088));
#31973=CARTESIAN_POINT('Ctrl Pts',(-9.4383592010789,0.187997765394267,1.82833212146347));
#31974=CARTESIAN_POINT('Ctrl Pts',(-9.33920755218048,-1.25955421209835,
1.22333549611273));
#31975=CARTESIAN_POINT('Ctrl Pts',(-9.2770690766196,-1.55155841947111,0.350189761838226));
#31976=CARTESIAN_POINT('Ctrl Pts',(-9.25194377439629,-1.55421089288766,
-0.00124746091003079));
#31977=CARTESIAN_POINT('Origin',(-20.9400562256037,0.,0.));
#31978=CARTESIAN_POINT('',(-10.7900562256037,-1.55530876292539,-0.00141549567407365));
#31979=CARTESIAN_POINT('',(-10.6519437743963,-1.55770803555897,0.000647550266795888));
#31980=CARTESIAN_POINT('',(-20.9400562256037,-1.5555,1.83293981223255E-13));
#31981=CARTESIAN_POINT('Ctrl Pts',(-10.7900562256037,-1.55530876292539,
-0.00141549567407357));
#31982=CARTESIAN_POINT('Ctrl Pts',(-10.7809836167307,-1.55645685696222,
-0.128090375998343));
#31983=CARTESIAN_POINT('Ctrl Pts',(-10.73489783452,-1.48442131297674,-0.770267129004551));
#31984=CARTESIAN_POINT('Ctrl Pts',(-10.6517988789718,-0.595236530522984,
-1.73891781272768));
#31985=CARTESIAN_POINT('Ctrl Pts',(-10.5407593589592,1.1368648842552,-1.44418832623659));
#31986=CARTESIAN_POINT('Ctrl Pts',(-10.4297198389465,1.83006722788652,0.170281026853745));
#31987=CARTESIAN_POINT('Ctrl Pts',(-10.3186803189338,0.850902723426497,
1.62914279360528));
#31988=CARTESIAN_POINT('Ctrl Pts',(-10.2076407989211,-0.905840595584799,
1.59924810522983));
#31989=CARTESIAN_POINT('Ctrl Pts',(-10.1314327678111,-1.54339980391117,
0.575724981289948));
#31990=CARTESIAN_POINT('Ctrl Pts',(-10.0922379100386,-1.55794234153255,
0.0308819577665884));
#31991=CARTESIAN_POINT('Ctrl Pts',(-10.0900562256037,-1.55780423998256,
0.000547110510323474));
#31992=CARTESIAN_POINT('Ctrl Pts',(-10.6519437743963,-1.55770803555897,
0.000647550266795966));
#31993=CARTESIAN_POINT('Ctrl Pts',(-10.6175473166661,-1.55519061705744,
-0.47769039247032));
#31994=CARTESIAN_POINT('Ctrl Pts',(-10.5461376855984,-1.06339243988215,
-1.47523026632046));
#31995=CARTESIAN_POINT('Ctrl Pts',(-10.4377148811931,0.633891526962291,
-1.72520231805252));
#31996=CARTESIAN_POINT('Ctrl Pts',(-10.3266753611805,1.79287047934082,-0.404668939352399));
#31997=CARTESIAN_POINT('Ctrl Pts',(-10.2156358411678,1.31347401748173,1.28566228519341));
#31998=CARTESIAN_POINT('Ctrl Pts',(-10.1045963211551,-0.366211903252911,
1.8011191931919));
#31999=CARTESIAN_POINT('Ctrl Pts',(-10.0166989655646,-1.43092008288472,
0.906265457554098));
#32000=CARTESIAN_POINT('Ctrl Pts',(-9.96581478331166,-1.55470322948288,
0.195180254354059));
#32001=CARTESIAN_POINT('Ctrl Pts',(-9.95194377439629,-1.5535960288726,0.000967876971002899));
#32002=CARTESIAN_POINT('Origin',(-20.9400562256037,0.,0.));
#32003=CARTESIAN_POINT('',(-11.4900562256037,-1.55305926288001,0.00041138631351628));
#32004=CARTESIAN_POINT('',(-11.3519437743963,-1.55549132498077,-0.00141421151383214));
#32005=CARTESIAN_POINT('',(-20.9400562256037,-1.5555,1.83293981223255E-13));
#32006=CARTESIAN_POINT('Ctrl Pts',(-11.4900562256037,-1.55305926288001,
0.000411386313516286));
#32007=CARTESIAN_POINT('Ctrl Pts',(-11.4697293234227,-1.55238359018918,
-0.284438289989754));
#32008=CARTESIAN_POINT('Ctrl Pts',(-11.4123892479042,-1.34098631575837,
-1.08890284854511));
#32009=CARTESIAN_POINT('Ctrl Pts',(-11.318035999048,-0.0491532482193918,
-1.83731479199404));
#32010=CARTESIAN_POINT('Ctrl Pts',(-11.2069964790353,1.51605673496666,-1.03909271148097));
#32011=CARTESIAN_POINT('Ctrl Pts',(-11.0959569590226,1.69585148053222,0.708681481814863));
#32012=CARTESIAN_POINT('Ctrl Pts',(-10.9849174390099,0.325929498694267,
1.80884262681183));
#32013=CARTESIAN_POINT('Ctrl Pts',(-10.8829505278703,-1.20556935877834,
1.30120052871543));
#32014=CARTESIAN_POINT('Ctrl Pts',(-10.8179967900682,-1.55177302189475,
0.388700259260363));
#32015=CARTESIAN_POINT('Ctrl Pts',(-10.7900562256037,-1.55530876292539,
-0.00141549567407357));
#32016=CARTESIAN_POINT('Ctrl Pts',(-11.3519437743963,-1.55549132498077,
-0.00141421151383192));
#32017=CARTESIAN_POINT('Ctrl Pts',(-11.3433061966958,-1.55659501205107,
-0.121978863546162));
#32018=CARTESIAN_POINT('Ctrl Pts',(-11.2976554456577,-1.48874725562481,
-0.757950576461866));
#32019=CARTESIAN_POINT('Ctrl Pts',(-11.214991521282,-0.615565745527372,
-1.73182571845486));
#32020=CARTESIAN_POINT('Ctrl Pts',(-11.1039520012693,1.11986930393965,-1.45740668595354));
#32021=CARTESIAN_POINT('Ctrl Pts',(-10.9929124812566,1.83193632103844,0.148831521622652));
#32022=CARTESIAN_POINT('Ctrl Pts',(-10.8818729612439,0.869928460211977,
1.61906330335833));
#32023=CARTESIAN_POINT('Ctrl Pts',(-10.7708334412312,-0.887044467963301,
1.60974955133526));
#32024=CARTESIAN_POINT('Ctrl Pts',(-10.6941903789487,-1.54025737311525,
0.587965478802919));
#32025=CARTESIAN_POINT('Ctrl Pts',(-10.6545604900037,-1.55789954854368,
0.0370371799838544));
#32026=CARTESIAN_POINT('Ctrl Pts',(-10.6519437743963,-1.55770803555897,
0.000647550266795966));
#32027=CARTESIAN_POINT('Origin',(-20.9400562256037,0.,0.));
#32028=CARTESIAN_POINT('',(-12.1900562256037,-1.5568114087742,0.00117013613562253));
#32029=CARTESIAN_POINT('',(-12.0519437743963,-1.55301668366533,0.00031493299472482));
#32030=CARTESIAN_POINT('',(-20.9400562256037,-1.5555,1.83293981223255E-13));
#32031=CARTESIAN_POINT('Ctrl Pts',(-12.1900562256037,-1.5568114087742,0.00117013613562249));
#32032=CARTESIAN_POINT('Ctrl Pts',(-12.1584750301148,-1.55312521236765,
-0.4386816463206));
#32033=CARTESIAN_POINT('Ctrl Pts',(-12.0898806612882,-1.12861437631865,
-1.4002653092897));
#32034=CARTESIAN_POINT('Ctrl Pts',(-11.9842731191242,0.501409935092548,
-1.76825613633351));
#32035=CARTESIAN_POINT('Ctrl Pts',(-11.8732335991115,1.75707289349663,-0.539292623378071));
#32036=CARTESIAN_POINT('Ctrl Pts',(-11.7621940790988,1.40707327733112,1.18249164010207));
#32037=CARTESIAN_POINT('Ctrl Pts',(-11.6511545590861,-0.228749431006459,
1.82368182107101));
#32038=CARTESIAN_POINT('Ctrl Pts',(-11.5604419412544,-1.39434711281995,
0.986039404245019));
#32039=CARTESIAN_POINT('Ctrl Pts',(-11.5067424967603,-1.55361391983816,
0.234243324664662));
#32040=CARTESIAN_POINT('Ctrl Pts',(-11.4900562256037,-1.55305926288001,
0.000411386313516286));
#32041=CARTESIAN_POINT('Ctrl Pts',(-12.0519437743963,-1.55301668366533,
0.000314932994724976));
#32042=CARTESIAN_POINT('Ctrl Pts',(-12.0320519033878,-1.55251128218854,
-0.278457518785902));
#32043=CARTESIAN_POINT('Ctrl Pts',(-11.9751468590418,-1.34773454330521,
-1.07663970368379));
#32044=CARTESIAN_POINT('Ctrl Pts',(-11.8812286413582,-0.0706725909392507,
-1.83661288546561));
#32045=CARTESIAN_POINT('Ctrl Pts',(-11.7701891213455,1.50378050738072,-1.05678081539653));
#32046=CARTESIAN_POINT('Ctrl Pts',(-11.6591496013328,1.70403672974556,0.688767253755881));
#32047=CARTESIAN_POINT('Ctrl Pts',(-11.5481100813201,0.34709631401335,1.80490045569464));
#32048=CARTESIAN_POINT('Ctrl Pts',(-11.4457081390079,-1.19680295565656,
1.31314440998192));
#32049=CARTESIAN_POINT('Ctrl Pts',(-11.3803193700333,-1.55186556564147,
0.394656762641098));
#32050=CARTESIAN_POINT('Ctrl Pts',(-11.3519437743963,-1.55549132498077,
-0.00141421151383192));
#32051=CARTESIAN_POINT('Origin',(-20.9400562256037,0.,0.));
#32052=CARTESIAN_POINT('',(-12.8900562256037,-1.55666010321292,-0.00122146201820818));
#32053=CARTESIAN_POINT('',(-12.7519437743963,-1.55664245885653,0.00122697214749692));
#32054=CARTESIAN_POINT('',(-20.9400562256037,-1.5555,1.83293981223255E-13));
#32055=CARTESIAN_POINT('Ctrl Pts',(-12.8900562256037,-1.55666010321292,
-0.00122146201820782));
#32056=CARTESIAN_POINT('Ctrl Pts',(-12.8842339101444,-1.55735948147068,
-0.0823331232632712));
#32057=CARTESIAN_POINT('Ctrl Pts',(-12.8413984213475,-1.51473567899467,
-0.678344946172016));
#32058=CARTESIAN_POINT('Ctrl Pts',(-12.761549759213,-0.744960386131938,
-1.68023085014673));
#32059=CARTESIAN_POINT('Ctrl Pts',(-12.6505102392003,1.00627386240032,-1.53803595554219));
#32060=CARTESIAN_POINT('Ctrl Pts',(-12.5394707191877,1.83794678447648,0.00965940594506788));
#32061=CARTESIAN_POINT('Ctrl Pts',(-12.4284311991749,0.990052298275348,
1.5485277309013));
#32062=CARTESIAN_POINT('Ctrl Pts',(-12.3173916791622,-0.762579793343959,
1.67230790988804));
#32063=CARTESIAN_POINT('Ctrl Pts',(-12.2379333546385,-1.5180706132219,0.667323369933976));
#32064=CARTESIAN_POINT('Ctrl Pts',(-12.1954882034523,-1.55744543598299,
0.0768248129769098));
#32065=CARTESIAN_POINT('Ctrl Pts',(-12.1900562256037,-1.5568114087742,0.00117013613562249));
#32066=CARTESIAN_POINT('Ctrl Pts',(-12.7519437743963,-1.55664245885653,
0.00122697214749681));
#32067=CARTESIAN_POINT('Ctrl Pts',(-12.7207976100799,-1.55289025223912,
-0.432688241818353));
#32068=CARTESIAN_POINT('Ctrl Pts',(-12.6526382724259,-1.13824355650797,
-1.38854277671179));
#32069=CARTESIAN_POINT('Ctrl Pts',(-12.5474657614343,0.480661769934936,
-1.77400839036668));
#32070=CARTESIAN_POINT('Ctrl Pts',(-12.4364262414216,1.75063489249572,-0.559838351084378));
#32071=CARTESIAN_POINT('Ctrl Pts',(-12.3253867214089,1.42082866667544,1.16592770192737));
#32072=CARTESIAN_POINT('Ctrl Pts',(-12.2143472013962,-0.207370712553722,
1.82623626449135));
#32073=CARTESIAN_POINT('Ctrl Pts',(-12.123199552392,-1.38833725657031,0.998354084754823));
#32074=CARTESIAN_POINT('Ctrl Pts',(-12.0690650767254,-1.55345169209053,
0.240259552880984));
#32075=CARTESIAN_POINT('Ctrl Pts',(-12.0519437743963,-1.55301668366533,
0.000314932994724976));
#32076=CARTESIAN_POINT('Origin',(-20.9400562256037,0.,0.));
#32077=CARTESIAN_POINT('',(-13.5900562256037,-1.55302057111372,-0.000324920039265338));
#32078=CARTESIAN_POINT('',(-13.4519437743963,-1.55682839314694,-0.00116389690534152));
#32079=CARTESIAN_POINT('',(-20.9400562256037,-1.5555,1.83293981223255E-13));
#32080=CARTESIAN_POINT('Ctrl Pts',(-13.5900562256037,-1.55302057111372,
-0.000324920039265191));
#32081=CARTESIAN_POINT('Ctrl Pts',(-13.5729796168364,-1.55346826531772,
-0.239641713856127));
#32082=CARTESIAN_POINT('Ctrl Pts',(-13.5188898347316,-1.38895922343596,
-0.997089159776875));
#32083=CARTESIAN_POINT('Ctrl Pts',(-13.4277868792892,-0.209568452681189,
-1.82598541898106));
#32084=CARTESIAN_POINT('Ctrl Pts',(-13.3167473592765,1.4194244756517,-1.1676368633319));
#32085=CARTESIAN_POINT('Ctrl Pts',(-13.2057078392638,1.75130743978355,0.557731062474938));
#32086=CARTESIAN_POINT('Ctrl Pts',(-13.0946683192511,0.482796462927691,
1.77342867408733));
#32087=CARTESIAN_POINT('Ctrl Pts',(-12.9894511146977,-1.13725980242033,
1.38974871282814));
#32088=CARTESIAN_POINT('Ctrl Pts',(-12.9212470834819,-1.55291344812471,
0.433303653605542));
#32089=CARTESIAN_POINT('Ctrl Pts',(-12.8900562256037,-1.55666010321292,
-0.00122146201820782));
#32090=CARTESIAN_POINT('Ctrl Pts',(-13.4519437743963,-1.55682839314694,
-0.00116389690534121));
#32091=CARTESIAN_POINT('Ctrl Pts',(-13.4465564901095,-1.55745489713643,
-0.0761939586894047));
#32092=CARTESIAN_POINT('Ctrl Pts',(-13.4041560324851,-1.51844833398138,
-0.666061655826624));
#32093=CARTESIAN_POINT('Ctrl Pts',(-13.3247424015232,-0.764591851789241,
-1.67138888543208));
#32094=CARTESIAN_POINT('Ctrl Pts',(-13.2137028815105,0.988187893799185,
-1.54971810104841));
#32095=CARTESIAN_POINT('Ctrl Pts',(-13.1026633614978,1.83793377915969,-0.0118713770116975));
#32096=CARTESIAN_POINT('Ctrl Pts',(-12.9916238414851,1.00812414086676,1.53682374486147));
#32097=CARTESIAN_POINT('Ctrl Pts',(-12.8805843214724,-0.742937660327962,
1.68112615202868));
#32098=CARTESIAN_POINT('Ctrl Pts',(-12.8006909657761,-1.51434968958816,
0.679607163890773));
#32099=CARTESIAN_POINT('Ctrl Pts',(-12.7578107834174,-1.55734926274576,
0.08296366527229));
#32100=CARTESIAN_POINT('Ctrl Pts',(-12.7519437743963,-1.55664245885653,
0.00122697214749681));
#32101=CARTESIAN_POINT('Origin',(-20.9400562256037,0.,0.));
#32102=CARTESIAN_POINT('',(-14.2900562256037,-1.55547253832405,0.0014146944387468));
#32103=CARTESIAN_POINT('',(-14.1519437743963,-1.55306423282011,-0.000421191186355668));
#32104=CARTESIAN_POINT('',(-20.9400562256037,-1.5555,1.83293981223255E-13));
#32105=CARTESIAN_POINT('Ctrl Pts',(-14.2900562256037,-1.55547253832405,
0.00141469443874675));
#32106=CARTESIAN_POINT('Ctrl Pts',(-14.2617253235285,-1.55185529681908,
-0.394044692501087));
#32107=CARTESIAN_POINT('Ctrl Pts',(-14.1963812481157,-1.19770891737767,
-1.31191857440859));
#32108=CARTESIAN_POINT('Ctrl Pts',(-14.0940239993653,0.344923864904767,
-1.8053169289933));
#32109=CARTESIAN_POINT('Ctrl Pts',(-13.9829844793526,1.70320660624744,-0.690817590341849));
#32110=CARTESIAN_POINT('Ctrl Pts',(-13.8719449593399,1.50505129966774,1.05497027069917));
#32111=CARTESIAN_POINT('Ctrl Pts',(-13.7609054393273,-0.0684621685615409,
1.83669665926807));
#32112=CARTESIAN_POINT('Ctrl Pts',(-13.6669425280818,-1.34704602164299,
1.07790003576514));
#32113=CARTESIAN_POINT('Ctrl Pts',(-13.609992790174,-1.5524978979924,0.279072165043973));
#32114=CARTESIAN_POINT('Ctrl Pts',(-13.5900562256037,-1.55302057111372,
-0.000324920039265191));
#32115=CARTESIAN_POINT('Ctrl Pts',(-14.1519437743963,-1.55306423282011,
-0.000421191186355634));
#32116=CARTESIAN_POINT('Ctrl Pts',(-14.1353021968015,-1.5536306920086,-0.233624933925084));
#32117=CARTESIAN_POINT('Ctrl Pts',(-14.0816474458692,-1.39495898335225,
-0.984773952170566));
#32118=CARTESIAN_POINT('Ctrl Pts',(-13.9909795215993,-0.230944069595307,
-1.82340515050471));
#32119=CARTESIAN_POINT('Ctrl Pts',(-13.8799400015866,1.40564908600105,-1.18418417199048));
#32120=CARTESIAN_POINT('Ctrl Pts',(-13.7689004815739,1.75772061547503,0.537177572225828));
#32121=CARTESIAN_POINT('Ctrl Pts',(-13.6578609615613,0.503537663837979,
1.76765135908215));
#32122=CARTESIAN_POINT('Ctrl Pts',(-13.5522087258354,-1.12761832251555,
1.40146764598756));
#32123=CARTESIAN_POINT('Ctrl Pts',(-13.483569663447,-1.5531505204737,0.439297805712299));
#32124=CARTESIAN_POINT('Ctrl Pts',(-13.4519437743963,-1.55682839314694,
-0.00116389690534121));
#32125=CARTESIAN_POINT('Origin',(-20.9400562256037,0.,0.));
#32126=CARTESIAN_POINT('',(-14.9900562256037,-1.55771859828449,-0.000637424228261111));
#32127=CARTESIAN_POINT('',(-14.8519437743963,-1.55529006138918,0.00141519769127213));
#32128=CARTESIAN_POINT('',(-20.9400562256037,-1.5555,1.83293981223255E-13));
#32129=CARTESIAN_POINT('Ctrl Pts',(-14.9900562256037,-1.55771859828449,
-0.000637424228261464));
#32130=CARTESIAN_POINT('Ctrl Pts',(-14.9874842035581,-1.55790433195692,
-0.0364048781015495));
#32131=CARTESIAN_POINT('Ctrl Pts',(-14.9478990081749,-1.54058372170137,
-0.586707661205107));
#32132=CARTESIAN_POINT('Ctrl Pts',(-14.8713006394542,-0.888981191146498,
-1.60868086595148));
#32133=CARTESIAN_POINT('Ctrl Pts',(-14.7602611194415,0.867979302403128,
-1.62010913746279));
#32134=CARTESIAN_POINT('Ctrl Pts',(-14.6492215994288,1.83175592377073,-0.151036162628272));
#32135=CARTESIAN_POINT('Ctrl Pts',(-14.5381820794161,1.12162251930453,1.4560579009365));
#32136=CARTESIAN_POINT('Ctrl Pts',(-14.4271425594034,-0.613481054986446,
1.73256534706872));
#32137=CARTESIAN_POINT('Ctrl Pts',(-14.3444339414659,-1.48830675260198,
0.759215790299635));
#32138=CARTESIAN_POINT('Ctrl Pts',(-14.298738496866,-1.5565810759867,0.122606941036985));
#32139=CARTESIAN_POINT('Ctrl Pts',(-14.2900562256037,-1.55547253832405,
0.00141469443874675));
#32140=CARTESIAN_POINT('Ctrl Pts',(-14.8519437743963,-1.55529006138918,
0.00141519769127204));
#32141=CARTESIAN_POINT('Ctrl Pts',(-14.8240479034936,-1.5517644390058,-0.388088446331793));
#32142=CARTESIAN_POINT('Ctrl Pts',(-14.7591388592533,-1.20646344528897,
-1.29997195727927));
#32143=CARTESIAN_POINT('Ctrl Pts',(-14.6572166416755,0.323752302625325,
-1.80923352630697));
#32144=CARTESIAN_POINT('Ctrl Pts',(-14.5461771216628,1.6949973052892,-0.71072191554133));
#32145=CARTESIAN_POINT('Ctrl Pts',(-14.4351376016501,1.51730614988444,1.03726734918786));
#32146=CARTESIAN_POINT('Ctrl Pts',(-14.3240980816374,-0.0469419935946381,
1.8373725684808));
#32147=CARTESIAN_POINT('Ctrl Pts',(-14.2297001392195,-1.34028715463676,
1.09016214116502));
#32148=CARTESIAN_POINT('Ctrl Pts',(-14.1723153701391,-1.55237080832191,
0.285052487359556));
#32149=CARTESIAN_POINT('Ctrl Pts',(-14.1519437743963,-1.55306423282011,
-0.000421191186355634));
#32150=CARTESIAN_POINT('Origin',(-20.9400562256037,0.,0.));
#32151=CARTESIAN_POINT('',(-15.6900562256037,-1.55360798640993,-0.000975396588764602));
#32152=CARTESIAN_POINT('',(-15.5519437743963,-1.55781326646842,-0.000536565987746263));
#32153=CARTESIAN_POINT('',(-20.9400562256037,-1.5555,1.83293981223255E-13));
#32154=CARTESIAN_POINT('Ctrl Pts',(-15.6900562256037,-1.55360798640993,
-0.000975396588764697));
#32155=CARTESIAN_POINT('Ctrl Pts',(-15.6762299102502,-1.55472072171226,
-0.194558284943319));
#32156=CARTESIAN_POINT('Ctrl Pts',(-15.625390421559,-1.43146895103288,-0.904998367253485));
#32157=CARTESIAN_POINT('Ctrl Pts',(-15.5375377595304,-0.368379304064812,
-1.80067719900824));
#32158=CARTESIAN_POINT('Ctrl Pts',(-15.4264982395177,1.31192580014841,-1.28724216120951));
#32159=CARTESIAN_POINT('Ctrl Pts',(-15.315458719505,1.79335624998195,0.402510928225848));
#32160=CARTESIAN_POINT('Ctrl Pts',(-15.2044191994923,0.635967374718456,
1.72443822301191));
#32161=CARTESIAN_POINT('Ctrl Pts',(-15.0959517015252,-1.06231602123872,
1.47640683538839));
#32162=CARTESIAN_POINT('Ctrl Pts',(-15.0244973768957,-1.5552314961529,0.478313482231629));
#32163=CARTESIAN_POINT('Ctrl Pts',(-14.9900562256037,-1.55771859828449,
-0.000637424228261464));
#32164=CARTESIAN_POINT('Ctrl Pts',(-15.5519437743963,-1.55781326646842,
-0.000536565987745981));
#32165=CARTESIAN_POINT('Ctrl Pts',(-15.5498067835232,-1.55794626072305,
-0.0302495182367311));
#32166=CARTESIAN_POINT('Ctrl Pts',(-15.5106566193126,-1.54371834758075,
-0.574467772409033));
#32167=CARTESIAN_POINT('Ctrl Pts',(-15.4344932817643,-0.907764618603845,
-1.59815672053134));
#32168=CARTESIAN_POINT('Ctrl Pts',(-15.3234537617517,0.848941402803422,
-1.63016563599362));
#32169=CARTESIAN_POINT('Ctrl Pts',(-15.212414241739,1.82986091954754,-0.172483394218017));
#32170=CARTESIAN_POINT('Ctrl Pts',(-15.1013747217263,1.13860211855666,1.4428190190688));
#32171=CARTESIAN_POINT('Ctrl Pts',(-14.9903352017136,-0.593143287092892,
1.7396328771166));
#32172=CARTESIAN_POINT('Ctrl Pts',(-14.9071915526036,-1.48397203957219,
0.771532660500938));
#32173=CARTESIAN_POINT('Ctrl Pts',(-14.8610610768312,-1.55644235255271,
0.128717999400674));
#32174=CARTESIAN_POINT('Ctrl Pts',(-14.8519437743963,-1.55529006138918,
0.00141519769127204));
#32175=CARTESIAN_POINT('Origin',(-20.9400562256037,0.,0.));
#32176=CARTESIAN_POINT('',(-16.3900562256037,-1.55419531422885,0.00124249107025136));
#32177=CARTESIAN_POINT('',(-16.2519437743963,-1.55372892642411,-0.00104588007964812));
#32178=CARTESIAN_POINT('',(-20.9400562256037,-1.5555,1.83293981223255E-13));
#32179=CARTESIAN_POINT('Ctrl Pts',(-16.3900562256037,-1.55419531422885,
0.00124249107025116));
#32180=CARTESIAN_POINT('Ctrl Pts',(-16.3649756169422,-1.55155993342647,
-0.349578491669034));
#32181=CARTESIAN_POINT('Ctrl Pts',(-16.3028818349431,-1.26037345479531,
-1.22209225599236));
#32182=CARTESIAN_POINT('Ctrl Pts',(-16.2037748796065,0.185797227123519,
-1.82855710250446));
#32183=CARTESIAN_POINT('Ctrl Pts',(-16.0927353595938,1.63630140628791,-0.837053997341315));
#32184=CARTESIAN_POINT('Ctrl Pts',(-15.9816958395811,1.59150738893344,0.919372567381872));
#32185=CARTESIAN_POINT('Ctrl Pts',(-15.8706563195684,0.0923492065994037,
1.83565065051508));
#32186=CARTESIAN_POINT('Ctrl Pts',(-15.7734431149093,-1.29402133831582,
1.16924087449169));
#32187=CARTESIAN_POINT('Ctrl Pts',(-15.7132430835877,-1.55174191907607,
0.323664887220352));
#32188=CARTESIAN_POINT('Ctrl Pts',(-15.6900562256037,-1.55360798640993,
-0.000975396588764697));
#32189=CARTESIAN_POINT('Ctrl Pts',(-16.2519437743963,-1.55372892642411,
-0.00104588007964796));
#32190=CARTESIAN_POINT('Ctrl Pts',(-16.2385524902153,-1.55489017216451,
-0.188501220428145));
#32191=CARTESIAN_POINT('Ctrl Pts',(-16.1881480326967,-1.43676012847776,
-0.892664308505406));
#32192=CARTESIAN_POINT('Ctrl Pts',(-16.1007304018405,-0.38944755395593,
-1.79623832185249));
#32193=CARTESIAN_POINT('Ctrl Pts',(-15.9896908818278,1.29675670604634,-1.30252199654784));
#32194=CARTESIAN_POINT('Ctrl Pts',(-15.8786513618151,1.7979482560302,0.381475523206329));
#32195=CARTESIAN_POINT('Ctrl Pts',(-15.7676118418024,0.656124176779396,
1.71686999240324));
#32196=CARTESIAN_POINT('Ctrl Pts',(-15.6587093126628,-1.05177064300029,
1.48783477827668));
#32197=CARTESIAN_POINT('Ctrl Pts',(-15.5868199568608,-1.55564276964987,
0.484385647412444));
#32198=CARTESIAN_POINT('Ctrl Pts',(-15.5519437743963,-1.55781326646842,
-0.000536565987745981));
#32199=CARTESIAN_POINT('Origin',(-20.9400562256037,0.,0.));
#32200=CARTESIAN_POINT('',(-17.0900562256037,-1.55801584159885,0.000174956040060638));
#32201=CARTESIAN_POINT('',(-16.9519437743963,-1.55404711770872,0.00119070638040702));
#32202=CARTESIAN_POINT('',(-20.9400562256037,-1.5555,1.83293981223255E-13));
#32203=CARTESIAN_POINT('Ctrl Pts',(-17.0900562256037,-1.55801584159885,
0.000174956040060662));
#32204=CARTESIAN_POINT('Ctrl Pts',(-17.0537213236343,-1.55720986486587,
-0.504853817882453));
#32205=CARTESIAN_POINT('Ctrl Pts',(-16.9803732483272,-1.0155113961936,-1.52582327293244));
#32206=CARTESIAN_POINT('Ctrl Pts',(-16.8700119996827,0.723039919366596,
-1.68977956052457));
#32207=CARTESIAN_POINT('Ctrl Pts',(-16.7589724796699,1.81154203999908,-0.310575472322002));
#32208=CARTESIAN_POINT('Ctrl Pts',(-16.6479329596573,1.24460614954145,1.35244120715334));
#32209=CARTESIAN_POINT('Ctrl Pts',(-16.5368934396446,-0.459685807164506,
1.77955911551557));
#32210=CARTESIAN_POINT('Ctrl Pts',(-16.4509345282934,-1.45383630619501,
0.851306302953154));
#32211=CARTESIAN_POINT('Ctrl Pts',(-16.4019887902798,-1.55544914551719,
0.168152079380301));
#32212=CARTESIAN_POINT('Ctrl Pts',(-16.3900562256037,-1.55419531422885,
0.00124249107025116));
#32213=CARTESIAN_POINT('Ctrl Pts',(-16.9519437743963,-1.55404711770872,
0.00119070638040689));
#32214=CARTESIAN_POINT('Ctrl Pts',(-16.9272981969073,-1.55158138149309,
-0.34362803432111));
#32215=CARTESIAN_POINT('Ctrl Pts',(-16.8656394460808,-1.26828644052862,
-1.20998033778118));
#32216=CARTESIAN_POINT('Ctrl Pts',(-16.7669675219167,0.164364346776865,
-1.83060805961026));
#32217=CARTESIAN_POINT('Ctrl Pts',(-16.655928001904,1.62638365175698,-0.856164542273203));
#32218=CARTESIAN_POINT('Ctrl Pts',(-16.5448884818913,1.60216788290627,0.900666187385256));
#32219=CARTESIAN_POINT('Ctrl Pts',(-16.4338489618786,0.113846090200382,
1.83444285109954));
#32220=CARTESIAN_POINT('Ctrl Pts',(-16.3362007260469,-1.28647431282795,
1.18140975480378));
#32221=CARTESIAN_POINT('Ctrl Pts',(-16.2755656635528,-1.55168051808682,
0.329620634919902));
#32222=CARTESIAN_POINT('Ctrl Pts',(-16.2519437743963,-1.55372892642411,
-0.00104588007964796));
#32223=CARTESIAN_POINT('Origin',(-20.9400562256037,0.,0.));
#32224=CARTESIAN_POINT('',(-17.7900562256037,-1.55469842977811,-0.00136248394244802));
#32225=CARTESIAN_POINT('',(-17.6519437743963,-1.55797555090531,0.00028566433304557));
#32226=CARTESIAN_POINT('',(-20.9400562256037,-1.5555,1.83293981223255E-13));
#32227=CARTESIAN_POINT('Ctrl Pts',(-17.7900562256037,-1.55469842977811,
-0.00136248394244807));
#32228=CARTESIAN_POINT('Ctrl Pts',(-17.7794802036639,-1.55594593301098,
-0.149176061089705));
#32229=CARTESIAN_POINT('Ctrl Pts',(-17.7318910083865,-1.46881329755037,
-0.812855446110298));
#32230=CARTESIAN_POINT('Ctrl Pts',(-17.6472886397715,-0.524370017185474,
-1.76158383684904));
#32231=CARTESIAN_POINT('Ctrl Pts',(-17.5362491197588,1.19438366161834,-1.39699298808207));
#32232=CARTESIAN_POINT('Ctrl Pts',(-17.4252095997461,1.821676008134,0.244209379874806));
#32233=CARTESIAN_POINT('Ctrl Pts',(-17.3141700797334,0.784269631776072,
1.66224631422945));
#32234=CARTESIAN_POINT('Ctrl Pts',(-17.2031305597208,-0.96982436419101,
1.56127588796884));
#32235=CARTESIAN_POINT('Ctrl Pts',(-17.1284259416775,-1.55368629794985,
0.533471930190121));
#32236=CARTESIAN_POINT('Ctrl Pts',(-17.0907344969718,-1.5580308869385,0.00960243592468178));
#32237=CARTESIAN_POINT('Ctrl Pts',(-17.0900562256037,-1.55801584159885,
0.000174956040060662));
#32238=CARTESIAN_POINT('Ctrl Pts',(-17.6519437743963,-1.55797555090531,
0.000285664333045577));
#32239=CARTESIAN_POINT('Ctrl Pts',(-17.6160439035994,-1.55671161178009,
-0.498731121651786));
#32240=CARTESIAN_POINT('Ctrl Pts',(-17.5431308594649,-1.02647039901201,
-1.51454913854194));
#32241=CARTESIAN_POINT('Ctrl Pts',(-17.4332046419928,0.703195832570145,
-1.6981334271154));
#32242=CARTESIAN_POINT('Ctrl Pts',(-17.3221651219801,1.80777954461665,-0.331774961689621));
#32243=CARTESIAN_POINT('Ctrl Pts',(-17.2111256019674,1.26036351771076,1.33776877909999));
#32244=CARTESIAN_POINT('Ctrl Pts',(-17.1000860819547,-0.438808100203742,
1.78482182831828));
#32245=CARTESIAN_POINT('Ctrl Pts',(-17.013692139431,-1.44885012350902,0.86363987975288));
#32246=CARTESIAN_POINT('Ctrl Pts',(-16.9643113702449,-1.55528446866947,
0.174226977407924));
#32247=CARTESIAN_POINT('Ctrl Pts',(-16.9519437743963,-1.55404711770872,
0.00119070638040689));
#32248=CARTESIAN_POINT('Origin',(-20.9400562256037,0.,0.));
#32249=CARTESIAN_POINT('',(-18.4900562256037,-1.55329134941458,0.000728404769962799));
#32250=CARTESIAN_POINT('',(-18.3519437743963,-1.55487053919943,-0.00138677294343165));
#32251=CARTESIAN_POINT('',(-20.9400562256037,-1.5555,1.83293981223255E-13));
#32252=CARTESIAN_POINT('Ctrl Pts',(-18.4900562256037,-1.55329134941458,
0.000728404769962943));
#32253=CARTESIAN_POINT('Ctrl Pts',(-18.4682259103559,-1.5519987435958,-0.305075653610566));
#32254=CARTESIAN_POINT('Ctrl Pts',(-18.4093824217706,-1.31686688150724,
-1.13120485114901));
#32255=CARTESIAN_POINT('Ctrl Pts',(-18.3135257598477,0.0252485661867687,
-1.83779672371819));
#32256=CARTESIAN_POINT('Ctrl Pts',(-18.202486239835,1.5568693034731,-0.976883390785028));
#32257=CARTESIAN_POINT('Ctrl Pts',(-18.0914467198223,1.66577977622518,0.776737156863176));
#32258=CARTESIAN_POINT('Ctrl Pts',(-17.9804071998096,0.252453550943756,
1.820551509628));
#32259=CARTESIAN_POINT('Ctrl Pts',(-17.8799437017367,-1.2349855334043,1.25973428479012));
#32260=CARTESIAN_POINT('Ctrl Pts',(-17.8164933770014,-1.55158001417496,
0.368130879433178));
#32261=CARTESIAN_POINT('Ctrl Pts',(-17.7900562256037,-1.55469842977811,
-0.00136248394244807));
#32262=CARTESIAN_POINT('Ctrl Pts',(-18.3519437743963,-1.55487053919943,
-0.00138677294343177));
#32263=CARTESIAN_POINT('Ctrl Pts',(-18.341802783629,-1.55609861243653,-0.143080456376997));
#32264=CARTESIAN_POINT('Ctrl Pts',(-18.2946486195241,-1.47343564403532,
-0.800528910503304));
#32265=CARTESIAN_POINT('Ctrl Pts',(-18.2104812820817,-0.544969521563382,
-1.75532009416732));
#32266=CARTESIAN_POINT('Ctrl Pts',(-18.099441762069,1.17793694271932,-1.4108885006591));
#32267=CARTESIAN_POINT('Ctrl Pts',(-17.9884022420563,1.82441171535083,0.222853162755832));
#32268=CARTESIAN_POINT('Ctrl Pts',(-17.8773627220436,0.803687711301754,
1.6529450720079));
#32269=CARTESIAN_POINT('Ctrl Pts',(-17.7663232020309,-0.95146865288028,
1.57252947891983));
#32270=CARTESIAN_POINT('Ctrl Pts',(-17.6911835528151,-1.55080035464189,
0.545690517664059));
#32271=CARTESIAN_POINT('Ctrl Pts',(-17.6530570769369,-1.5580147473316,0.0157608357841803));
#32272=CARTESIAN_POINT('Ctrl Pts',(-17.6519437743963,-1.55797555090531,
0.000285664333045577));
#32273=CARTESIAN_POINT('Origin',(-20.9400562256037,0.,0.));
#32274=CARTESIAN_POINT('',(-19.1900562256037,-1.55732260026824,0.00102952447757971));
#32275=CARTESIAN_POINT('',(-19.0519437743963,-1.55320700821059,0.000650635102509151));
#32276=CARTESIAN_POINT('',(-20.9400562256037,-1.5555,1.83293981223255E-13));
#32277=CARTESIAN_POINT('Ctrl Pts',(-19.1900562256037,-1.55732260026824,
0.00102952447757978));
#32278=CARTESIAN_POINT('Ctrl Pts',(-19.156971617048,-1.5540834599925,-0.459324401254566));
#32279=CARTESIAN_POINT('Ctrl Pts',(-19.0868738351547,-1.09444465366423,
-1.44067331686593));
#32280=CARTESIAN_POINT('Ctrl Pts',(-18.9797628799239,0.572581864613586,
-1.74641810285352));
#32281=CARTESIAN_POINT('Ctrl Pts',(-18.8687233599111,1.7774511739937,-0.467787493561026));
#32282=CARTESIAN_POINT('Ctrl Pts',(-18.7576838398985,1.35806626263998,1.23849733645003));
#32283=CARTESIAN_POINT('Ctrl Pts',(-18.6466443198858,-0.302373835599965,
1.81291555390549));
#32284=CARTESIAN_POINT('Ctrl Pts',(-18.5574351151208,-1.41437165322348,
0.943454576583954));
#32285=CARTESIAN_POINT('Ctrl Pts',(-18.5052390836935,-1.55419034929111,
0.213413360024777));
#32286=CARTESIAN_POINT('Ctrl Pts',(-18.4900562256037,-1.55329134941458,
0.000728404769962943));
#32287=CARTESIAN_POINT('Ctrl Pts',(-19.0519437743963,-1.55320700821059,
0.000650635102509029));
#32288=CARTESIAN_POINT('Ctrl Pts',(-19.030548490321,-1.55209814412289,-0.29910286970105));
#32289=CARTESIAN_POINT('Ctrl Pts',(-18.9721400329082,-1.32398103540958,
-1.11899594634625));
#32290=CARTESIAN_POINT('Ctrl Pts',(-18.8767184021578,0.00372273104669908,
-1.83795501911246));
#32291=CARTESIAN_POINT('Ctrl Pts',(-18.7656788821451,1.54531676928027,-0.995059804671333));
#32292=CARTESIAN_POINT('Ctrl Pts',(-18.6546393621325,1.67476548588617,0.757173652727654));
#32293=CARTESIAN_POINT('Ctrl Pts',(-18.5435998421197,0.273761951577427,
1.81746760404448));
#32294=CARTESIAN_POINT('Ctrl Pts',(-18.4427013128744,-1.22661269048955,
1.27176249184623));
#32295=CARTESIAN_POINT('Ctrl Pts',(-18.3788159569665,-1.55161631986385,
0.374081326539656));
#32296=CARTESIAN_POINT('Ctrl Pts',(-18.3519437743963,-1.55487053919943,
-0.00138677294343177));
#32297=CARTESIAN_POINT('Ctrl Pts',(-19.8760740822721,-0.685825729128707,
1.39614588036676));
#32298=CARTESIAN_POINT('Ctrl Pts',(-19.8390609089345,-1.14966653079063,
1.1682943639365));
#32299=CARTESIAN_POINT('Ctrl Pts',(-19.7650345622594,-1.82446514616035,
0.217992868365382));
#32300=CARTESIAN_POINT('Ctrl Pts',(-19.6539950422467,-1.1726414776927,-1.41687333944346));
#32301=CARTESIAN_POINT('Ctrl Pts',(-19.542955522234,0.552287169619636,-1.75246537632802));
#32302=CARTESIAN_POINT('Ctrl Pts',(-19.4319160022213,1.77174315090552,-0.488859491694061));
#32303=CARTESIAN_POINT('Ctrl Pts',(-19.3208764822086,1.37253690144282,1.22265204623408));
#32304=CARTESIAN_POINT('Ctrl Pts',(-19.2098369621959,-0.281145520007231,
1.81625519837393));
#32305=CARTESIAN_POINT('Ctrl Pts',(-19.0987974421832,-1.67779713459217,
0.750436187074751));
#32306=CARTESIAN_POINT('Ctrl Pts',(-18.9877579221705,-1.541289524424,-1.00132217474655));
#32307=CARTESIAN_POINT('Ctrl Pts',(-18.8767184021578,0.00372273104669908,
-1.83795501911246));
#32308=CARTESIAN_POINT('Ctrl Pts',(-18.7656788821451,1.54531676928027,-0.995059804671333));
#32309=CARTESIAN_POINT('Ctrl Pts',(-18.6546393621325,1.67476548588617,0.757173652727654));
#32310=CARTESIAN_POINT('Ctrl Pts',(-18.5435998421197,0.273761951577427,
1.81746760404448));
#32311=CARTESIAN_POINT('Ctrl Pts',(-18.4325603221071,-1.3774105812666,1.21691540392665));
#32312=CARTESIAN_POINT('Ctrl Pts',(-18.3215208020943,-1.76986786954587,
-0.495691858702389));
#32313=CARTESIAN_POINT('Ctrl Pts',(-18.2104812820817,-0.544969521563382,
-1.75532009416732));
#32314=CARTESIAN_POINT('Ctrl Pts',(-18.099441762069,1.17793694271932,-1.4108885006591));
#32315=CARTESIAN_POINT('Ctrl Pts',(-17.9884022420563,1.82441171535083,0.222853162755832));
#32316=CARTESIAN_POINT('Ctrl Pts',(-17.8773627220436,0.803687711301754,
1.6529450720079));
#32317=CARTESIAN_POINT('Ctrl Pts',(-17.7663232020309,-0.95146865288028,
1.57252947891983));
#32318=CARTESIAN_POINT('Ctrl Pts',(-17.6552836820182,-1.83714625700249,
0.0550921927705897));
#32319=CARTESIAN_POINT('Ctrl Pts',(-17.5442441620055,-1.0439879835733,-1.5126898472865));
#32320=CARTESIAN_POINT('Ctrl Pts',(-17.4332046419928,0.703195832570145,
-1.6981334271154));
#32321=CARTESIAN_POINT('Ctrl Pts',(-17.3221651219801,1.80777954461665,-0.331774961689621));
#32322=CARTESIAN_POINT('Ctrl Pts',(-17.2111256019674,1.26036351771076,1.33776877909999));
#32323=CARTESIAN_POINT('Ctrl Pts',(-17.1000860819547,-0.438808100203742,
1.78482182831828));
#32324=CARTESIAN_POINT('Ctrl Pts',(-16.9890465619421,-1.7369845485084,0.600854545137668));
#32325=CARTESIAN_POINT('Ctrl Pts',(-16.8780070419293,-1.44785571598004,
-1.13219050140136));
#32326=CARTESIAN_POINT('Ctrl Pts',(-16.7669675219167,0.164364346776865,
-1.83060805961026));
#32327=CARTESIAN_POINT('Ctrl Pts',(-16.655928001904,1.62638365175698,-0.856164542273203));
#32328=CARTESIAN_POINT('Ctrl Pts',(-16.5448884818913,1.60216788290627,0.900666187385256));
#32329=CARTESIAN_POINT('Ctrl Pts',(-16.4338489618786,0.113846090200382,
1.83444285109954));
#32330=CARTESIAN_POINT('Ctrl Pts',(-16.3228094418659,-1.47851145821767,
1.09185409926492));
#32331=CARTESIAN_POINT('Ctrl Pts',(-16.2117699218532,-1.71976369772685,
-0.648501603808868));
#32332=CARTESIAN_POINT('Ctrl Pts',(-16.1007304018405,-0.38944755395593,
-1.79623832185249));
#32333=CARTESIAN_POINT('Ctrl Pts',(-15.9896908818278,1.29675670604634,-1.30252199654784));
#32334=CARTESIAN_POINT('Ctrl Pts',(-15.8786513618151,1.7979482560302,0.381475523206329));
#32335=CARTESIAN_POINT('Ctrl Pts',(-15.7676118418024,0.656124176779396,
1.71686999240324));
#32336=CARTESIAN_POINT('Ctrl Pts',(-15.6565723217897,-1.0852846088457,1.48334042753872));
#32337=CARTESIAN_POINT('Ctrl Pts',(-15.545532801777,-1.83492982812703,-0.105707294062363));
#32338=CARTESIAN_POINT('Ctrl Pts',(-15.4344932817643,-0.907764618603845,
-1.59815672053134));
#32339=CARTESIAN_POINT('Ctrl Pts',(-15.3234537617517,0.848941402803422,
-1.63016563599362));
#32340=CARTESIAN_POINT('Ctrl Pts',(-15.212414241739,1.82986091954754,-0.172483394218017));
#32341=CARTESIAN_POINT('Ctrl Pts',(-15.1013747217263,1.13860211855666,1.4428190190688));
#32342=CARTESIAN_POINT('Ctrl Pts',(-14.9903352017136,-0.593143287092892,
1.7396328771166));
#32343=CARTESIAN_POINT('Ctrl Pts',(-14.8792956817009,-1.78285769279516,
0.446721337535475));
#32344=CARTESIAN_POINT('Ctrl Pts',(-14.7682561616882,-1.3433466499118,-1.25441671080192));
#32345=CARTESIAN_POINT('Ctrl Pts',(-14.6572166416755,0.323752302625325,
-1.80923352630697));
#32346=CARTESIAN_POINT('Ctrl Pts',(-14.5461771216628,1.6949973052892,-0.71072191554133));
#32347=CARTESIAN_POINT('Ctrl Pts',(-14.4351376016501,1.51730614988444,1.03726734918786));
#32348=CARTESIAN_POINT('Ctrl Pts',(-14.3240980816374,-0.0469419935946381,
1.8373725684808));
#32349=CARTESIAN_POINT('Ctrl Pts',(-14.2130585616247,-1.56829322450421,
0.958435114205744));
#32350=CARTESIAN_POINT('Ctrl Pts',(-14.102019041612,-1.65649404608369,-0.796347274408376));
#32351=CARTESIAN_POINT('Ctrl Pts',(-13.9909795215993,-0.230944069595307,
-1.82340515050471));
#32352=CARTESIAN_POINT('Ctrl Pts',(-13.8799400015866,1.40564908600105,-1.18418417199048));
#32353=CARTESIAN_POINT('Ctrl Pts',(-13.7689004815739,1.75772061547503,0.537177572225828));
#32354=CARTESIAN_POINT('Ctrl Pts',(-13.6578609615613,0.503537663837979,
1.76765135908215));
#32355=CARTESIAN_POINT('Ctrl Pts',(-13.5468214415485,-1.21079215177004,
1.38279567231766));
#32356=CARTESIAN_POINT('Ctrl Pts',(-13.4357819215359,-1.81866608220935,
-0.265697549084784));
#32357=CARTESIAN_POINT('Ctrl Pts',(-13.3247424015232,-0.764591851789241,
-1.67138888543208));
#32358=CARTESIAN_POINT('Ctrl Pts',(-13.2137028815105,0.988187893799185,
-1.54971810104841));
#32359=CARTESIAN_POINT('Ctrl Pts',(-13.1026633614978,1.83793377915969,-0.0118713770116975));
#32360=CARTESIAN_POINT('Ctrl Pts',(-12.9916238414851,1.00812414086676,1.53682374486147));
#32361=CARTESIAN_POINT('Ctrl Pts',(-12.8805843214724,-0.742937660327962,
1.68112615202868));
#32362=CARTESIAN_POINT('Ctrl Pts',(-12.7695448014597,-1.81508215488039,
0.289168250683079));
#32363=CARTESIAN_POINT('Ctrl Pts',(-12.658505281447,-1.22855358205609,-1.36703972224128));
#32364=CARTESIAN_POINT('Ctrl Pts',(-12.5474657614343,0.480661769934936,
-1.77400839036668));
#32365=CARTESIAN_POINT('Ctrl Pts',(-12.4364262414216,1.75063489249572,-0.559838351084378));
#32366=CARTESIAN_POINT('Ctrl Pts',(-12.3253867214089,1.42082866667544,1.16592770192737));
#32367=CARTESIAN_POINT('Ctrl Pts',(-12.2143472013962,-0.207370712553722,
1.82623626449135));
#32368=CARTESIAN_POINT('Ctrl Pts',(-12.1033076813836,-1.64606890862666,
0.817678820944377));
#32369=CARTESIAN_POINT('Ctrl Pts',(-11.9922681613708,-1.58054309013141,
-0.938096501649056));
#32370=CARTESIAN_POINT('Ctrl Pts',(-11.8812286413582,-0.0706725909392507,
-1.83661288546561));
#32371=CARTESIAN_POINT('Ctrl Pts',(-11.7701891213455,1.50378050738072,-1.05678081539653));
#32372=CARTESIAN_POINT('Ctrl Pts',(-11.6591496013328,1.70403672974556,0.688767253755881));
#32373=CARTESIAN_POINT('Ctrl Pts',(-11.5481100813201,0.34709631401335,1.80490045569464));
#32374=CARTESIAN_POINT('Ctrl Pts',(-11.4370705613074,-1.32703046504225,
1.2716649130247));
#32375=CARTESIAN_POINT('Ctrl Pts',(-11.3260310412947,-1.78847952257671,
-0.423653754252368));
#32376=CARTESIAN_POINT('Ctrl Pts',(-11.214991521282,-0.615565745527372,
-1.73182571845486));
#32377=CARTESIAN_POINT('Ctrl Pts',(-11.1039520012693,1.11986930393965,-1.45740668595354));
#32378=CARTESIAN_POINT('Ctrl Pts',(-10.9929124812566,1.83193632103844,0.148831521622652));
#32379=CARTESIAN_POINT('Ctrl Pts',(-10.8818729612439,0.869928460211977,
1.61906330335833));
#32380=CARTESIAN_POINT('Ctrl Pts',(-10.7708334412312,-0.887044467963301,
1.60974955133526));
#32381=CARTESIAN_POINT('Ctrl Pts',(-10.6597939212185,-1.83341124003695,
0.129401433819494));
#32382=CARTESIAN_POINT('Ctrl Pts',(-10.5487544012059,-1.10435531176706,
-1.46919734941914));
#32383=CARTESIAN_POINT('Ctrl Pts',(-10.4377148811931,0.633891526962291,
-1.72520231805252));
#32384=CARTESIAN_POINT('Ctrl Pts',(-10.3266753611805,1.79287047934082,-0.404668939352399));
#32385=CARTESIAN_POINT('Ctrl Pts',(-10.2156358411678,1.31347401748173,1.28566228519341));
#32386=CARTESIAN_POINT('Ctrl Pts',(-10.1045963211551,-0.366211903252911,
1.8011191931919));
#32387=CARTESIAN_POINT('Ctrl Pts',(-9.99355680114238,-1.71124309816971,
0.670662780490254));
#32388=CARTESIAN_POINT('Ctrl Pts',(-9.88251728112968,-1.49249227306246,
-1.07266412311459));
#32389=CARTESIAN_POINT('Ctrl Pts',(-9.77147776111699,0.0901399223399556,
-1.83576041480606));
#32390=CARTESIAN_POINT('Ctrl Pts',(-9.66043824110429,1.59039972425115,-0.921287264250532));
#32391=CARTESIAN_POINT('Ctrl Pts',(-9.54939872109161,1.63730757628732,0.835084071696088));
#32392=CARTESIAN_POINT('Ctrl Pts',(-9.4383592010789,0.187997765394267,1.82833212146347));
#32393=CARTESIAN_POINT('Ctrl Pts',(-9.32731968106623,-1.43310968526294,
1.15079891213624));
#32394=CARTESIAN_POINT('Ctrl Pts',(-9.21628016105352,-1.74460124269406,
-0.578366674488338));
#32395=CARTESIAN_POINT('Ctrl Pts',(-9.10524064104083,-0.461827170446667,
-1.77900454490864));
#32396=CARTESIAN_POINT('Ctrl Pts',(-8.99420112102814,1.24297754506556,-1.35393808153518));
#32397=CARTESIAN_POINT('Ctrl Pts',(-8.88316160101544,1.81191445877564,0.308395039272923));
#32398=CARTESIAN_POINT('Ctrl Pts',(-8.77212208100275,0.725073034805075,
1.68890810891739));
#32399=CARTESIAN_POINT('Ctrl Pts',(-8.66108256099006,-1.0243604991031,1.52604949921214));
#32400=CARTESIAN_POINT('Ctrl Pts',(-8.55004304097736,-1.83770462979697,
-0.0313560168251536));
#32401=CARTESIAN_POINT('Ctrl Pts',(-8.43900352096468,-0.971702639962959,
-1.56010752374873));
#32402=CARTESIAN_POINT('Ctrl Pts',(-8.32796400095197,0.782268521994644,
-1.66318894466765));
#32403=CARTESIAN_POINT('Ctrl Pts',(-8.2169244809393,1.82138073092891,-0.246401581101293));
#32404=CARTESIAN_POINT('Ctrl Pts',(-8.10588496092658,1.1960640567365,1.39555446986186));
#32405=CARTESIAN_POINT('Ctrl Pts',(-7.99484544091391,-0.522249555601089,
1.76221363853615));
#32406=CARTESIAN_POINT('Ctrl Pts',(-7.8838059209012,-1.76331685156899,0.518512475395882));
#32407=CARTESIAN_POINT('Ctrl Pts',(-7.77276640088852,-1.39301566865845,
-1.19901995523027));
#32408=CARTESIAN_POINT('Ctrl Pts',(-7.66172688087582,0.250262368674325,
-1.82085426462248));
#32409=CARTESIAN_POINT('Ctrl Pts',(-7.55068736086313,1.66484362245829,-0.778740790589749));
#32410=CARTESIAN_POINT('Ctrl Pts',(-7.43964784085044,1.55804400070415,0.97500789639785));
#32411=CARTESIAN_POINT('Ctrl Pts',(-7.32860832083774,0.0274599982776329,
1.83776697507137));
#32412=CARTESIAN_POINT('Ctrl Pts',(-7.21756880082506,-1.52821772205629,
1.02112296035368));
#32413=CARTESIAN_POINT('Ctrl Pts',(-7.10652928081235,-1.68736715310754,
-0.728651903711305));
#32414=CARTESIAN_POINT('Ctrl Pts',(-6.99548976079967,-0.304553073520857,
-1.8125641868848));
#32415=CARTESIAN_POINT('Ctrl Pts',(-6.88445024078697,1.35657016098623,-1.24010439257756));
#32416=CARTESIAN_POINT('Ctrl Pts',(-6.77341072077428,1.77802146990873,0.465597636067849));
#32417=CARTESIAN_POINT('Ctrl Pts',(-6.66237120076158,0.574666806591611,
1.74582346403357));
#32418=CARTESIAN_POINT('Ctrl Pts',(-6.55133168074889,-1.15383452969896,
1.43066676212274));
#32419=CARTESIAN_POINT('Ctrl Pts',(-6.4402921607362,-1.82792945607851,-0.191873421215389));
#32420=CARTESIAN_POINT('Ctrl Pts',(-6.3292526407235,-0.831611090304988,
-1.6390742816145));
#32421=CARTESIAN_POINT('Ctrl Pts',(-6.21821312071081,0.924656853680087,
-1.58844301412132));
#32422=CARTESIAN_POINT('Ctrl Pts',(-6.10717360069812,1.83594738678564,-0.0862478934429835));
#32423=CARTESIAN_POINT('Ctrl Pts',(-5.99613408068542,1.06949761739632,1.49476297537502));
#32424=CARTESIAN_POINT('Ctrl Pts',(-5.88509456067274,-0.674289122018889,
1.70981744232983));
#32425=CARTESIAN_POINT('Ctrl Pts',(-5.77405504066003,-1.80189151776093,
0.362392693620539));
#32426=CARTESIAN_POINT('Ctrl Pts',(-5.66301552064736,-1.28287482091343,
-1.31619667984489));
#32427=CARTESIAN_POINT('Ctrl Pts',(-5.55197600063464,0.408468929309301,
-1.79200854907483));
#32428=CARTESIAN_POINT('Ctrl Pts',(-5.44093648062197,1.726542296104,-0.630232660159929));
#32429=CARTESIAN_POINT('Ctrl Pts',(-5.32989696060926,1.46685280597546,1.1074675398269));
#32430=CARTESIAN_POINT('Ctrl Pts',(-5.21885744059658,-0.133287989090187,
1.83313278791599));
#32431=CARTESIAN_POINT('Ctrl Pts',(-5.10781792058388,-1.61162647503488,
0.8836297930327));
#32432=CARTESIAN_POINT('Ctrl Pts',(-4.99677840057119,-1.61721540987848,
-0.873358932066274));
#32433=CARTESIAN_POINT('Ctrl Pts',(-4.8857388805585,-0.144947467941284,
-1.83224772825777));
#32434=CARTESIAN_POINT('Ctrl Pts',(-4.7746993605458,1.45977754246094,-1.11677707385809));
#32435=CARTESIAN_POINT('Ctrl Pts',(-4.66365984053311,1.73051682250325,0.619235846185912));
#32436=CARTESIAN_POINT('Ctrl Pts',(-4.55262032052042,0.419861211735448,
1.78937365271996));
#32437=CARTESIAN_POINT('Ctrl Pts',(-4.44158080050772,-1.27447537020456,
1.324331543425));
#32438=CARTESIAN_POINT('Ctrl Pts',(-4.33054128049503,-1.80416055280736,
-0.350921936991871));
#32439=CARTESIAN_POINT('Ctrl Pts',(-4.21950176048233,-0.685153134847353,
-1.70549309232754));
#32440=CARTESIAN_POINT('Ctrl Pts',(-4.10846224046965,1.0599664669302,-1.50153674452297));
#32441=CARTESIAN_POINT('Ctrl Pts',(-3.99742272045695,1.83645893175252,0.0745660657000111));
#32442=CARTESIAN_POINT('Ctrl Pts',(-3.88638320044426,0.93474362991831,1.5825283101715));
#32443=CARTESIAN_POINT('Ctrl Pts',(-3.77534368043157,-0.821166662308707,
1.64433172410147));
#32444=CARTESIAN_POINT('Ctrl Pts',(-3.66430416041887,-1.82667178805772,
0.20349861148378));
#32445=CARTESIAN_POINT('Ctrl Pts',(-3.55326464040618,-1.1629129140303,-1.42329724953858));
#32446=CARTESIAN_POINT('Ctrl Pts',(-3.44222512039348,0.563548452575144,
-1.74944409679311));
#32447=CARTESIAN_POINT('Ctrl Pts',(-3.3311856003808,1.77502341045502,-0.476899778205122));
#32448=CARTESIAN_POINT('Ctrl Pts',(-3.22014608036809,1.36443210709099,1.23144895602193));
#32449=CARTESIAN_POINT('Ctrl Pts',(-3.10910656035541,-0.293015589158281,
1.81446503711471));
#32450=CARTESIAN_POINT('Ctrl Pts',(-2.99806704034271,-1.68269740770543,
0.739371990178813));
#32451=CARTESIAN_POINT('Ctrl Pts',(-2.88702752033002,-1.53468306041474,
-1.01137995345248));
#32452=CARTESIAN_POINT('Ctrl Pts',(-2.77598800031732,0.0157677844803547,
-1.83790448190824));
#32453=CARTESIAN_POINT('Ctrl Pts',(-2.66494848030463,1.55180958399743,-0.984900257957451));
#32454=CARTESIAN_POINT('Ctrl Pts',(-2.55390896029194,1.66976418974896,0.768133489551486));
#32455=CARTESIAN_POINT('Ctrl Pts',(-2.44286944027925,0.261841363970268,
1.81922527888795));
#32456=CARTESIAN_POINT('Ctrl Pts',(-2.33182992026655,-1.38535945017504,
1.20785788805628));
#32457=CARTESIAN_POINT('Ctrl Pts',(-2.22079040025386,-1.76657988960961,
-0.507283956920983));
#32458=CARTESIAN_POINT('Ctrl Pts',(-2.10975088024117,-0.533449971191177,
-1.75885550507193));
#32459=CARTESIAN_POINT('Ctrl Pts',(-1.99871136022847,1.18716147401266,-1.40313541149553));
#32460=CARTESIAN_POINT('Ctrl Pts',(-1.88767184021578,1.82291149503699,0.234809115073605));
#32461=CARTESIAN_POINT('Ctrl Pts',(-1.77663232020309,0.792833618333258,
1.65817871653077));
#32462=CARTESIAN_POINT('Ctrl Pts',(-1.66559280019039,-0.96175759007224,
1.56625756194791));
#32463=CARTESIAN_POINT('Ctrl Pts',(-1.5545532801777,-1.83746826916603,0.0430471165426282));
#32464=CARTESIAN_POINT('Ctrl Pts',(-1.44351376016501,-1.03404772328313,
-1.51950265405236));
#32465=CARTESIAN_POINT('Ctrl Pts',(-1.33247424015232,0.714312595491066,
-1.69348504977325));
#32466=CARTESIAN_POINT('Ctrl Pts',(-1.22143472013962,1.8099179685225,-0.319919240308951));
#32467=CARTESIAN_POINT('Ctrl Pts',(-1.11039520012693,1.25156189493757,1.34600919589416));
#32468=CARTESIAN_POINT('Ctrl Pts',(-0.999355680114236,-0.45049222129505,
1.78189485367676));
#32469=CARTESIAN_POINT('Ctrl Pts',(-0.888316160101544,-1.74090124670998,
0.589476331112601));
#32470=CARTESIAN_POINT('Ctrl Pts',(-0.77727664008885,-1.44037375318949,
-1.14170098836771));
#32471=CARTESIAN_POINT('Ctrl Pts',(-0.66623712007616,0.17630871353902,-1.82941001051451));
#32472=CARTESIAN_POINT('Ctrl Pts',(-0.555197600063458,1.63206374948406,
-0.84563791873513));
#32473=CARTESIAN_POINT('Ctrl Pts',(-0.444158080050773,1.59603445699364,
0.91144468152982));
#32474=CARTESIAN_POINT('Ctrl Pts',(-0.333118560038075,0.102187466450462,
1.83458816486299));
#32475=CARTESIAN_POINT('Ctrl Pts',(-0.222079040025385,-1.48635127732985,
1.08322572698902));
#32476=CARTESIAN_POINT('Ctrl Pts',(-0.111039520012692,-1.71404440126355,
-0.662001322286585));
#32477=CARTESIAN_POINT('Ctrl Pts',(-0.0370131733375646,-0.825376844998173,
-1.41612072810435));
#32478=CARTESIAN_POINT('Ctrl Pts',(0.,-0.319621170202026,-1.52230829911641));
#32479=CARTESIAN_POINT('Ctrl Pts',(-19.7993827215147,-0.744392439309325,
1.51537102412035));
#32480=CARTESIAN_POINT('Ctrl Pts',(-19.7623695481771,-1.24784334693123,
1.26806192078395));
#32481=CARTESIAN_POINT('Ctrl Pts',(-19.688343201502,-1.98026700210055,0.236608567078233));
#32482=CARTESIAN_POINT('Ctrl Pts',(-19.5773036814893,-1.27278026026218,
-1.53786852336466));
#32483=CARTESIAN_POINT('Ctrl Pts',(-19.4662641614766,0.599450233391951,
-1.90211874661982));
#32484=CARTESIAN_POINT('Ctrl Pts',(-19.3552246414639,1.92304276424226,-0.530606091381193));
#32485=CARTESIAN_POINT('Ctrl Pts',(-19.2441851214512,1.48974593502792,1.32706152666359));
#32486=CARTESIAN_POINT('Ctrl Pts',(-19.1331456014385,-0.305154196686319,
1.9713559583765));
#32487=CARTESIAN_POINT('Ctrl Pts',(-19.0221060814259,-1.8210741426571,0.814520365913112));
#32488=CARTESIAN_POINT('Ctrl Pts',(-18.9110665614131,-1.67290934130666,
-1.08683099005494));
#32489=CARTESIAN_POINT('Ctrl Pts',(-18.8000270414005,0.00404063704095619,
-1.99490885498866));
#32490=CARTESIAN_POINT('Ctrl Pts',(-18.6889875213878,1.67728049639015,-1.08003383920717));
#32491=CARTESIAN_POINT('Ctrl Pts',(-18.5779480013751,1.81778360356014,0.821833183556338));
#32492=CARTESIAN_POINT('Ctrl Pts',(-18.4669084813624,0.297140101733544,
1.97267189852895));
#32493=CARTESIAN_POINT('Ctrl Pts',(-18.3558689613497,-1.4950358071607,1.32083499858318));
#32494=CARTESIAN_POINT('Ctrl Pts',(-18.244829441337,-1.92100734153001,-0.538021914567167));
#32495=CARTESIAN_POINT('Ctrl Pts',(-18.1337899213243,-0.591507688142816,
-1.90521724567824));
#32496=CARTESIAN_POINT('Ctrl Pts',(-18.0227504013116,1.27852793632774,-1.53137260384405));
#32497=CARTESIAN_POINT('Ctrl Pts',(-17.9117108812989,1.98020900851858,0.241883910716462));
#32498=CARTESIAN_POINT('Ctrl Pts',(-17.8006713612862,0.872319352350435,
1.79409981564771));
#32499=CARTESIAN_POINT('Ctrl Pts',(-17.6896318412736,-1.03272018147192,
1.7068170600512));
#32500=CARTESIAN_POINT('Ctrl Pts',(-17.5785923212608,-1.99403102790477,
0.0597968405406536));
#32501=CARTESIAN_POINT('Ctrl Pts',(-17.4675528012482,-1.13314028432416,
-1.64186736880022));
#32502=CARTESIAN_POINT('Ctrl Pts',(-17.3565132812354,0.763245878488775,
-1.84314707132529));
#32503=CARTESIAN_POINT('Ctrl Pts',(-17.2454737612228,1.96215651847923,-0.360107185461877));
#32504=CARTESIAN_POINT('Ctrl Pts',(-17.1344342412101,1.36799340345118,1.45200875734308));
#32505=CARTESIAN_POINT('Ctrl Pts',(-17.0233947211974,-0.47628051591815,
1.93723830717499));
#32506=CARTESIAN_POINT('Ctrl Pts',(-16.9123552011847,-1.8853159194675,0.65216506399276));
#32507=CARTESIAN_POINT('Ctrl Pts',(-16.801315681172,-1.57149666804647,-1.22887493616156));
#32508=CARTESIAN_POINT('Ctrl Pts',(-16.6902761611593,0.178400389247811,
-1.98693449521611));
#32509=CARTESIAN_POINT('Ctrl Pts',(-16.5792366411466,1.76527015882334,-0.929277489899003));
#32510=CARTESIAN_POINT('Ctrl Pts',(-16.4681971211339,1.73898646242799,0.977579393358277));
#32511=CARTESIAN_POINT('Ctrl Pts',(-16.3571576011212,0.123568080331052,
1.99109676220276));
#32512=CARTESIAN_POINT('Ctrl Pts',(-16.2461180811085,-1.60477028519716,
1.18509397037967));
#32513=CARTESIAN_POINT('Ctrl Pts',(-16.1350785610958,-1.86662447851419,
-0.703880986454943));
#32514=CARTESIAN_POINT('Ctrl Pts',(-16.0240390410831,-0.422704781053617,
-1.94962972252928));
#32515=CARTESIAN_POINT('Ctrl Pts',(-15.9129995210704,1.4074944211132,-1.41375204382615));
#32516=CARTESIAN_POINT('Ctrl Pts',(-15.8019600010578,1.95148567808699,0.414051971507585));
#32517=CARTESIAN_POINT('Ctrl Pts',(-15.690920481045,0.712154495957904,1.86348366259991));
#32518=CARTESIAN_POINT('Ctrl Pts',(-15.5798809610324,-1.17796347236763,
1.61001162873322));
#32519=CARTESIAN_POINT('Ctrl Pts',(-15.4688414410197,-1.99162532507519,
-0.114734264315));
#32520=CARTESIAN_POINT('Ctrl Pts',(-15.357801921007,-0.985284001548998,
-1.73463276320396));
#32521=CARTESIAN_POINT('Ctrl Pts',(-15.2467624009943,0.921437523882869,
-1.7693751090341));
#32522=CARTESIAN_POINT('Ctrl Pts',(-15.1357228809816,1.98612355245008,-0.187212770109111));
#32523=CARTESIAN_POINT('Ctrl Pts',(-15.0246833609689,1.23583407917913,1.56602985783425));
#32524=CARTESIAN_POINT('Ctrl Pts',(-14.9136438409562,-0.643795296073198,
1.88819040449921));
#32525=CARTESIAN_POINT('Ctrl Pts',(-14.8026043209435,-1.93510644251742,
0.484869511329067));
#32526=CARTESIAN_POINT('Ctrl Pts',(-14.6915648009308,-1.45806295549196,
-1.36153876357265));
#32527=CARTESIAN_POINT('Ctrl Pts',(-14.5805252809181,0.351399424150296,
-1.96373466425475));
#32528=CARTESIAN_POINT('Ctrl Pts',(-14.4694857609054,1.8397431375313,-0.77141465814138));
#32529=CARTESIAN_POINT('Ctrl Pts',(-14.3584462408927,1.64687788474545,1.12584573526981));
#32530=CARTESIAN_POINT('Ctrl Pts',(-14.2474067208801,-0.0509506477139025,
1.99427666545703));
#32531=CARTESIAN_POINT('Ctrl Pts',(-14.1363672008673,-1.7022190468475,1.04028155008079));
#32532=CARTESIAN_POINT('Ctrl Pts',(-14.0253276808547,-1.79795185758359,
-0.864352072190827));
#32533=CARTESIAN_POINT('Ctrl Pts',(-13.914288160842,-0.250665747883883,
-1.97911648715448));
#32534=CARTESIAN_POINT('Ctrl Pts',(-13.8032486408293,1.52568576461917,-1.2853086534087));
#32535=CARTESIAN_POINT('Ctrl Pts',(-13.6922091208166,1.90782276168028,0.583050338224345));
#32536=CARTESIAN_POINT('Ctrl Pts',(-13.5811696008039,0.546537719348393,
1.91860155014488));
#32537=CARTESIAN_POINT('Ctrl Pts',(-13.4701300807912,-1.31418884575491,
1.50088076294629));
#32538=CARTESIAN_POINT('Ctrl Pts',(-13.3590905607785,-1.97397272182371,
-0.288387032275693));
#32539=CARTESIAN_POINT('Ctrl Pts',(-13.2480510407658,-0.829884866455036,
-1.81411865524772));
#32540=CARTESIAN_POINT('Ctrl Pts',(-13.1370115207531,1.07257509527332,-1.6820576838766));
#32541=CARTESIAN_POINT('Ctrl Pts',(-13.0259720007404,1.99488580123086,-0.0128851440188925));
#32542=CARTESIAN_POINT('Ctrl Pts',(-12.9149324807277,1.09421381624131,1.66806220244796));
#32543=CARTESIAN_POINT('Ctrl Pts',(-12.803892960715,-0.806381495673676,
1.824687444557));
#32544=CARTESIAN_POINT('Ctrl Pts',(-12.6928534407024,-1.97008274176989,
0.313862035724786));
#32545=CARTESIAN_POINT('Ctrl Pts',(-12.5818139206897,-1.33346702948977,
-1.48377931922258));
#32546=CARTESIAN_POINT('Ctrl Pts',(-12.470774400677,0.521708317737177,-1.92550144588175));
#32547=CARTESIAN_POINT('Ctrl Pts',(-12.3597348806643,1.90013194696043,-0.607646254846737));
#32548=CARTESIAN_POINT('Ctrl Pts',(-12.2486953606516,1.54216161935306,1.26549315552602));
#32549=CARTESIAN_POINT('Ctrl Pts',(-12.1376558406389,-0.225079322636813,
1.98218936668781));
#32550=CARTESIAN_POINT('Ctrl Pts',(-12.0266163206262,-1.78663645605788,
0.88750524549088));
#32551=CARTESIAN_POINT('Ctrl Pts',(-11.9155768006135,-1.71551500086051,
-1.0182061032578));
#32552=CARTESIAN_POINT('Ctrl Pts',(-11.8045372806008,-0.0767077409422943,
-1.99345210862173));
#32553=CARTESIAN_POINT('Ctrl Pts',(-11.6934977605881,1.63219720773243,-1.14702557162399));
#32554=CARTESIAN_POINT('Ctrl Pts',(-11.5824582405754,1.84955449183783,0.747585158099991));
#32555=CARTESIAN_POINT('Ctrl Pts',(-11.4714187205627,0.376736918563704,
1.95903156714741));
#32556=CARTESIAN_POINT('Ctrl Pts',(-11.36037920055,-1.44035343521676,1.38025989166828));
#32557=CARTESIAN_POINT('Ctrl Pts',(-11.2493396805373,-1.94120835355214,
-0.459832050849315));
#32558=CARTESIAN_POINT('Ctrl Pts',(-11.1383001605246,-0.668132540682749,
-1.8797165464425));
#32559=CARTESIAN_POINT('Ctrl Pts',(-11.027260640512,1.21550155886733,-1.58186325176356));
#32560=CARTESIAN_POINT('Ctrl Pts',(-10.9162211204993,1.98837618473367,0.161541124401333));
#32561=CARTESIAN_POINT('Ctrl Pts',(-10.8051816004866,0.944216790093985,
1.75732468263366));
#32562=CARTESIAN_POINT('Ctrl Pts',(-10.6941420804739,-0.962794434851429,
1.74721557430902));
#32563=CARTESIAN_POINT('Ctrl Pts',(-10.5831025604612,-1.98997705577781,
0.140451786627161));
#32564=CARTESIAN_POINT('Ctrl Pts',(-10.4720630404485,-1.19866273526199,
-1.59466078962992));
#32565=CARTESIAN_POINT('Ctrl Pts',(-10.3610235204358,0.688023268844763,
-1.87252753475538));
#32566=CARTESIAN_POINT('Ctrl Pts',(-10.2499840004231,1.9459742800517,-0.439226010461765));
#32567=CARTESIAN_POINT('Ctrl Pts',(-10.1389444804104,1.42563932252114,1.39545258212894));
#32568=CARTESIAN_POINT('Ctrl Pts',(-10.0279049603977,-0.39748490088419,
1.95492740030364));
#32569=CARTESIAN_POINT('Ctrl Pts',(-9.91686544038502,-1.85737625462972,
0.727934636919118));
#32570=CARTESIAN_POINT('Ctrl Pts',(-9.80582592037233,-1.61994500440615,
-1.16426524881077));
#32571=CARTESIAN_POINT('Ctrl Pts',(-9.69478640035963,0.0978375027648033,
-1.99252684045702));
#32572=CARTESIAN_POINT('Ctrl Pts',(-9.58374688034695,1.72621335119086,-0.999961425785681));
#32573=CARTESIAN_POINT('Ctrl Pts',(-9.47270736033424,1.77712694179689,0.906396833417073));
#32574=CARTESIAN_POINT('Ctrl Pts',(-9.36166784032156,0.204052005083444,
1.98446420126701));
#32575=CARTESIAN_POINT('Ctrl Pts',(-9.25062832030885,-1.5554913866617,1.24907242900888));
#32576=CARTESIAN_POINT('Ctrl Pts',(-9.13958880029619,-1.89358304816144,
-0.627756821232938));
#32577=CARTESIAN_POINT('Ctrl Pts',(-9.02854928028346,-0.501265320542654,
-1.93092425157233));
#32578=CARTESIAN_POINT('Ctrl Pts',(-8.9175097602708,1.34912273990295,-1.4695588520252));
#32579=CARTESIAN_POINT('Ctrl Pts',(-8.80647024025808,1.96664453738317,0.334730713364926));
#32580=CARTESIAN_POINT('Ctrl Pts',(-8.6954307202454,0.786991304251073,1.83313394871245));
#32581=CARTESIAN_POINT('Ctrl Pts',(-8.5843912002327,-1.11183669301559,1.65636788031917));
#32582=CARTESIAN_POINT('Ctrl Pts',(-8.47335168022002,-1.99463708345048,
-0.0340336923217584));
#32583=CARTESIAN_POINT('Ctrl Pts',(-8.36231216020732,-1.05468206823365,
-1.6933343207516));
#32584=CARTESIAN_POINT('Ctrl Pts',(-8.25127264019463,0.849071051945344,
-1.80521847310438));
#32585=CARTESIAN_POINT('Ctrl Pts',(-8.14023312018193,1.97691919043286,-0.267443267604836));
#32586=CARTESIAN_POINT('Ctrl Pts',(-8.02919360016924,1.29820303168762,1.51472910957899));
#32587=CARTESIAN_POINT('Ctrl Pts',(-7.91815408015655,-0.566847530080274,
1.91269947052086));
#32588=CARTESIAN_POINT('Ctrl Pts',(-7.80711456014386,-1.91389689343126,
0.56279131852139));
#32589=CARTESIAN_POINT('Ctrl Pts',(-7.69607504013116,-1.51197350514412,
-1.30141135181429));
#32590=CARTESIAN_POINT('Ctrl Pts',(-7.58503552011847,0.271633750634426,
-1.97634776605868));
#32591=CARTESIAN_POINT('Ctrl Pts',(-7.47399600010577,1.80701445360575,-0.845242066717456));
#32592=CARTESIAN_POINT('Ctrl Pts',(-7.36295648009308,1.69109458128501,1.05826958003969));
#32593=CARTESIAN_POINT('Ctrl Pts',(-7.25191696008039,0.0298049697366587,
1.99470475275613));
#32594=CARTESIAN_POINT('Ctrl Pts',(-7.1408774400677,-1.6587212605197,1.1083226817082));
#32595=CARTESIAN_POINT('Ctrl Pts',(-7.02983792005499,-1.83146140158355,
-0.790875793913607));
#32596=CARTESIAN_POINT('Ctrl Pts',(-6.91879840004232,-0.330560659462779,
-1.96734974961353));
#32597=CARTESIAN_POINT('Ctrl Pts',(-6.8077588800296,1.47241570028829,-1.34600423195228));
#32598=CARTESIAN_POINT('Ctrl Pts',(-6.69671936001693,1.92985722599114,0.505357768495393));
#32599=CARTESIAN_POINT('Ctrl Pts',(-6.58567984000423,0.623740999761369,
1.8949096422008));
#32600=CARTESIAN_POINT('Ctrl Pts',(-6.47464031999154,-1.2523672758867,1.5528398478842));
#32601=CARTESIAN_POINT('Ctrl Pts',(-6.36360079997884,-1.98402714990627,
-0.208258626048653));
#32602=CARTESIAN_POINT('Ctrl Pts',(-6.25256127996616,-0.902627273630063,
-1.77904451652791));
#32603=CARTESIAN_POINT('Ctrl Pts',(-6.14152175995345,1.00361876436081,-1.72408954602473));
#32604=CARTESIAN_POINT('Ctrl Pts',(-6.03048223994077,1.99272977907838,-0.0936131105300822));
#32605=CARTESIAN_POINT('Ctrl Pts',(-5.91944271992807,1.16082833646465,1.62240961540223));
#32606=CARTESIAN_POINT('Ctrl Pts',(-5.80840319991538,-0.731870653171702,
1.85582885361632));
#32607=CARTESIAN_POINT('Ctrl Pts',(-5.69736367990268,-1.95576567822975,
0.393339546381216));
#32608=CARTESIAN_POINT('Ctrl Pts',(-5.58632415988999,-1.39242707980852,
-1.42859448910627));
#32609=CARTESIAN_POINT('Ctrl Pts',(-5.4752846398773,0.443350504007648,-1.94503874446888));
#32610=CARTESIAN_POINT('Ctrl Pts',(-5.3642451198646,1.87398194144794,-0.684051949793199));
#32611=CARTESIAN_POINT('Ctrl Pts',(-5.25320559985191,1.59211603177235,1.20204073485982));
#32612=CARTESIAN_POINT('Ctrl Pts',(-5.14216607983922,-0.144670237810325,
1.98967482498543));
#32613=CARTESIAN_POINT('Ctrl Pts',(-5.03112655982653,-1.74925277961036,
0.959088160658));
#32614=CARTESIAN_POINT('Ctrl Pts',(-4.92008703981383,-1.75531898661405,
-0.94794021020374));
#32615=CARTESIAN_POINT('Ctrl Pts',(-4.80904751980114,-0.157325388432984,
-1.98871418485495));
#32616=CARTESIAN_POINT('Ctrl Pts',(-4.69800799978845,1.58443656971279,-1.21214526499329));
#32617=CARTESIAN_POINT('Ctrl Pts',(-4.58696847977575,1.87829587613392,0.67211605291583));
#32618=CARTESIAN_POINT('Ctrl Pts',(-4.47592895976307,0.455715640724303,
1.94217883874994));
#32619=CARTESIAN_POINT('Ctrl Pts',(-4.36488943975036,-1.38331035038812,
1.43742403674008));
#32620=CARTESIAN_POINT('Ctrl Pts',(-4.25384991973768,-1.95822847958197,
-0.380889234086341));
#32621=CARTESIAN_POINT('Ctrl Pts',(-4.14281039972498,-0.743662408229242,
-1.85113522182343));
#32622=CARTESIAN_POINT('Ctrl Pts',(-4.03177087971229,1.15048326475978,-1.62976183671034));
#32623=CARTESIAN_POINT('Ctrl Pts',(-3.92073135969959,1.99328500789168,0.0809337025116572));
#32624=CARTESIAN_POINT('Ctrl Pts',(-3.80969183968691,1.01456691000454,1.71766975056653));
#32625=CARTESIAN_POINT('Ctrl Pts',(-3.6986523196742,-0.891290934232011,
1.78475092308452));
#32626=CARTESIAN_POINT('Ctrl Pts',(-3.58761279966152,-1.98266208218415,
0.220876559983982));
#32627=CARTESIAN_POINT('Ctrl Pts',(-3.47657327964882,-1.26222091708206,
-1.54484100908882));
#32628=CARTESIAN_POINT('Ctrl Pts',(-3.36553375963613,0.61167318381939,-1.89883946217874));
#32629=CARTESIAN_POINT('Ctrl Pts',(-3.25449423962344,1.92660314453117,-0.517625067311445));
#32630=CARTESIAN_POINT('Ctrl Pts',(-3.14345471961074,1.4809490244114,1.33660965654155));
#32631=CARTESIAN_POINT('Ctrl Pts',(-3.03241519959805,-0.318037921158636,
1.96941292467288));
#32632=CARTESIAN_POINT('Ctrl Pts',(-2.92137567958535,-1.8263928790374,0.802511331888053));
#32633=CARTESIAN_POINT('Ctrl Pts',(-2.81033615957267,-1.66573871231129,
-1.09774766189583));
#32634=CARTESIAN_POINT('Ctrl Pts',(-2.69929663955997,0.0171142887374011,
-1.99485400211406));
#32635=CARTESIAN_POINT('Ctrl Pts',(-2.58825711954728,1.68432777090903,-1.06900670878697));
#32636=CARTESIAN_POINT('Ctrl Pts',(-2.47721759953459,1.81235521720314,0.833728945586275));
#32637=CARTESIAN_POINT('Ctrl Pts',(-2.36617807952189,0.284201544735738,
1.97457967160987));
#32638=CARTESIAN_POINT('Ctrl Pts',(-2.2551385595092,-1.50366347693917,1.31100400792993));
#32639=CARTESIAN_POINT('Ctrl Pts',(-2.14409903949651,-1.91743858156491,
-0.550603930527132));
#32640=CARTESIAN_POINT('Ctrl Pts',(-2.03305951948381,-0.579004415318382,
-1.90905456620366));
#32641=CARTESIAN_POINT('Ctrl Pts',(-1.92201999947112,1.2885402048375,-1.52295743259934));
#32642=CARTESIAN_POINT('Ctrl Pts',(-1.81098047945842,1.97858067553034,0.254860852426422));
#32643=CARTESIAN_POINT('Ctrl Pts',(-1.69994095944573,0.860538364268268,
1.79978039199151));
#32644=CARTESIAN_POINT('Ctrl Pts',(-1.58890143943304,-1.04388775178742,
1.70000954704084));
#32645=CARTESIAN_POINT('Ctrl Pts',(-1.47786191942035,-1.99438053858907,
0.0467231641033586));
#32646=CARTESIAN_POINT('Ctrl Pts',(-1.36682239940765,-1.12235116649073,
-1.64926196137903));
#32647=CARTESIAN_POINT('Ctrl Pts',(-1.25578287939496,0.775311967462195,
-1.83810174158394));
#32648=CARTESIAN_POINT('Ctrl Pts',(-1.14474335938227,1.96447755503407,-0.347239034000803));
#32649=CARTESIAN_POINT('Ctrl Pts',(-1.03370383936957,1.35844015811823,1.46095287200342));
#32650=CARTESIAN_POINT('Ctrl Pts',(-0.922664319356883,-0.488962413127507,
1.9340613808792));
#32651=CARTESIAN_POINT('Ctrl Pts',(-0.811624799344187,-1.88956708766444,
0.639815197061019));
#32652=CARTESIAN_POINT('Ctrl Pts',(-0.700585279331496,-1.56337577625731,
-1.23919757978839));
#32653=CARTESIAN_POINT('Ctrl Pts',(-0.589545759318804,0.191364756043121,
-1.9856341376312));
#32654=CARTESIAN_POINT('Ctrl Pts',(-0.478506239306104,1.77143531364765,
-0.917851935796283));
#32655=CARTESIAN_POINT('Ctrl Pts',(-0.367466719293418,1.73232926704656,
0.989278326786373));
#32656=CARTESIAN_POINT('Ctrl Pts',(-0.25642719928072,0.110913857831672,
1.99125448516684));
#32657=CARTESIAN_POINT('Ctrl Pts',(-0.14538767926803,-1.61327959277311,
1.17572877042737));
#32658=CARTESIAN_POINT('Ctrl Pts',(-0.0343481592553372,-1.86041677754202,
-0.718533525636265));
#32659=CARTESIAN_POINT('Ctrl Pts',(0.0396781874197904,-0.895860649290834,
-1.53705164209763));
#32660=CARTESIAN_POINT('Ctrl Pts',(0.0766913607573549,-0.346915509926753,
-1.65230719704803));
#32661=CARTESIAN_POINT('Ctrl Pts',(-19.7226913607574,-0.802959149489944,
1.63459616787394));
#32662=CARTESIAN_POINT('Ctrl Pts',(-19.6856781874198,-1.34602016307183,
1.3678294776314));
#32663=CARTESIAN_POINT('Ctrl Pts',(-19.6116518407446,-2.13606885804074,
0.255224265791084));
#32664=CARTESIAN_POINT('Ctrl Pts',(-19.500612320732,-1.37291904283165,-1.65886370728586));
#32665=CARTESIAN_POINT('Ctrl Pts',(-19.3895728007193,0.646613297164265,
-2.05177211691162));
#32666=CARTESIAN_POINT('Ctrl Pts',(-19.2785332807066,2.07434237757899,-0.572352691068324));
#32667=CARTESIAN_POINT('Ctrl Pts',(-19.1674937606939,1.60695496861303,1.43147100709311));
#32668=CARTESIAN_POINT('Ctrl Pts',(-19.0564542406812,-0.329162873365406,
2.12645671837908));
#32669=CARTESIAN_POINT('Ctrl Pts',(-18.9454147206685,-1.96435115072204,
0.878604544751473));
#32670=CARTESIAN_POINT('Ctrl Pts',(-18.8343752006558,-1.80452915818932,
-1.17233980536332));
#32671=CARTESIAN_POINT('Ctrl Pts',(-18.7233356806431,0.00435854303521161,
-2.15186269086486));
#32672=CARTESIAN_POINT('Ctrl Pts',(-18.6122961606304,1.80924422350002,-1.165007873743));
#32673=CARTESIAN_POINT('Ctrl Pts',(-18.5012566406177,1.96080172123412,0.886492714385021));
#32674=CARTESIAN_POINT('Ctrl Pts',(-18.390217120605,0.320518251889661,2.12787619301341));
#32675=CARTESIAN_POINT('Ctrl Pts',(-18.2791776005923,-1.6126610330548,1.42475459323971));
#32676=CARTESIAN_POINT('Ctrl Pts',(-18.1681380805797,-2.07214681351415,
-0.580351970431944));
#32677=CARTESIAN_POINT('Ctrl Pts',(-18.0570985605669,-0.63804585472225,
-2.05511439718916));
#32678=CARTESIAN_POINT('Ctrl Pts',(-17.9460590405543,1.37911892993617,-1.65185670702901));
#32679=CARTESIAN_POINT('Ctrl Pts',(-17.8350195205416,2.13600630168632,0.260914658677094));
#32680=CARTESIAN_POINT('Ctrl Pts',(-17.7239800005289,0.940950993399115,
1.93525455928752));
#32681=CARTESIAN_POINT('Ctrl Pts',(-17.6129404805162,-1.11397171006355,
1.84110464118256));
#32682=CARTESIAN_POINT('Ctrl Pts',(-17.5019009605035,-2.15091579880705,
0.0645014883107155));
#32683=CARTESIAN_POINT('Ctrl Pts',(-17.3908614404908,-1.22229258507502,
-1.77104489031393));
#32684=CARTESIAN_POINT('Ctrl Pts',(-17.2798219204781,0.823295924407405,
-1.98816071553518));
#32685=CARTESIAN_POINT('Ctrl Pts',(-17.1687824004654,2.11653349234182,-0.388439409234132));
#32686=CARTESIAN_POINT('Ctrl Pts',(-17.0577428804527,1.4756232891916,1.56624873558618));
#32687=CARTESIAN_POINT('Ctrl Pts',(-16.94670336044,-0.513752931632555,2.08965478603169));
#32688=CARTESIAN_POINT('Ctrl Pts',(-16.8356638404273,-2.0336472904266,0.70347558284785));
#32689=CARTESIAN_POINT('Ctrl Pts',(-16.7246243204146,-1.6951376201129,-1.32555937092177));
#32690=CARTESIAN_POINT('Ctrl Pts',(-16.613584800402,0.192436431718756,-2.14326093082196));
#32691=CARTESIAN_POINT('Ctrl Pts',(-16.5025452803892,1.90415666588971,-1.0023904375248));
#32692=CARTESIAN_POINT('Ctrl Pts',(-16.3915057603766,1.87580504194971,1.0544925993313));
#32693=CARTESIAN_POINT('Ctrl Pts',(-16.2804662403639,0.133290070461722,
2.14775067330598));
#32694=CARTESIAN_POINT('Ctrl Pts',(-16.1694267203512,-1.73102911217666,
1.27833384149443));
#32695=CARTESIAN_POINT('Ctrl Pts',(-16.0583872003385,-2.01348525930153,
-0.75926036910102));
#32696=CARTESIAN_POINT('Ctrl Pts',(-15.9473476803258,-0.455962008151305,
-2.10302112320607));
#32697=CARTESIAN_POINT('Ctrl Pts',(-15.8363081603131,1.51823213618007,-1.52498209110447));
#32698=CARTESIAN_POINT('Ctrl Pts',(-15.7252686403004,2.10502310014378,0.446628419808841));
#32699=CARTESIAN_POINT('Ctrl Pts',(-15.6142291202877,0.768184815136414,
2.01009733279657));
#32700=CARTESIAN_POINT('Ctrl Pts',(-15.503189600275,-1.27064233588956,1.73668282992772));
#32701=CARTESIAN_POINT('Ctrl Pts',(-15.3921500802623,-2.14832082202336,
-0.12376123456764));
#32702=CARTESIAN_POINT('Ctrl Pts',(-15.2811105602496,-1.06280338449415,
-1.87110880587658));
#32703=CARTESIAN_POINT('Ctrl Pts',(-15.1700710402369,0.993933644962316,
-1.90858458207459));
#32704=CARTESIAN_POINT('Ctrl Pts',(-15.0590315202243,2.14238618535262,-0.201942146000205));
#32705=CARTESIAN_POINT('Ctrl Pts',(-14.9479920002115,1.33306603980161,1.6892406965997));
#32706=CARTESIAN_POINT('Ctrl Pts',(-14.8369524801989,-0.694447305053506,
2.03674793188182));
#32707=CARTESIAN_POINT('Ctrl Pts',(-14.7259129601861,-2.08735519223967,
0.523017685122661));
#32708=CARTESIAN_POINT('Ctrl Pts',(-14.6148734401735,-1.57277926107211,
-1.46866081634339));
#32709=CARTESIAN_POINT('Ctrl Pts',(-14.5038339201608,0.379046545675268,
-2.11823580220253));
#32710=CARTESIAN_POINT('Ctrl Pts',(-14.3927944001481,1.9844889697734,-0.832107400741434));
#32711=CARTESIAN_POINT('Ctrl Pts',(-14.2817548801354,1.77644961960646,1.21442412135177));
#32712=CARTESIAN_POINT('Ctrl Pts',(-14.1707153601227,-0.0549593018331681,
2.15118076243326));
#32713=CARTESIAN_POINT('Ctrl Pts',(-14.05967584011,-1.83614486919079,1.12212798595584));
#32714=CARTESIAN_POINT('Ctrl Pts',(-13.9486363200973,-1.9394096690835,-0.932356869973282));
#32715=CARTESIAN_POINT('Ctrl Pts',(-13.8375968000846,-0.270387426172459,
-2.13482782380425));
#32716=CARTESIAN_POINT('Ctrl Pts',(-13.7265572800719,1.6457224432373,-1.38643313482693));
#32717=CARTESIAN_POINT('Ctrl Pts',(-13.6155177600592,2.05792490788552,0.628923104222863));
#32718=CARTESIAN_POINT('Ctrl Pts',(-13.5044782400466,0.589537774858808,
2.06955174120762));
#32719=CARTESIAN_POINT('Ctrl Pts',(-13.3934387200338,-1.41758553973979,
1.61896585357493));
#32720=CARTESIAN_POINT('Ctrl Pts',(-13.2823992000212,-2.12927936143807,
-0.311076515466602));
#32721=CARTESIAN_POINT('Ctrl Pts',(-13.1713596800084,-0.895177881120831,
-1.95684842506337));
#32722=CARTESIAN_POINT('Ctrl Pts',(-13.0603201599958,1.15696229674745,-1.81439726670479));
#32723=CARTESIAN_POINT('Ctrl Pts',(-12.9492806399831,2.15183782330204,-0.0138989110260861));
#32724=CARTESIAN_POINT('Ctrl Pts',(-12.8382411199704,1.18030349161586,1.79930066003444));
#32725=CARTESIAN_POINT('Ctrl Pts',(-12.7272015999577,-0.869825331019388,
1.96824873708532));
#32726=CARTESIAN_POINT('Ctrl Pts',(-12.616162079945,-2.12508332865939,0.33855582076649));
#32727=CARTESIAN_POINT('Ctrl Pts',(-12.5051225599323,-1.43838047692345,
-1.60051891620387));
#32728=CARTESIAN_POINT('Ctrl Pts',(-12.3940830399196,0.562754865539417,
-2.07699450139683));
#32729=CARTESIAN_POINT('Ctrl Pts',(-12.2830435199069,2.04962900142514,-0.655454158609094));
#32730=CARTESIAN_POINT('Ctrl Pts',(-12.1720039998942,1.66349457203068,1.36505860912468));
#32731=CARTESIAN_POINT('Ctrl Pts',(-12.0609644798815,-0.242787932719905,
2.13814246888428));
#32732=CARTESIAN_POINT('Ctrl Pts',(-11.9499249598688,-1.92720400348909,
0.957331670037384));
#32733=CARTESIAN_POINT('Ctrl Pts',(-11.8388854398561,-1.85048691158961,
-1.09831570486655));
#32734=CARTESIAN_POINT('Ctrl Pts',(-11.7278459198435,-0.0827428909453353,
-2.15029133177786));
#32735=CARTESIAN_POINT('Ctrl Pts',(-11.6168063998307,1.76061390808414,-1.23727032785145));
#32736=CARTESIAN_POINT('Ctrl Pts',(-11.5057668798181,1.9950722539301,0.806403062444103));
#32737=CARTESIAN_POINT('Ctrl Pts',(-11.3947273598054,0.406377523114059,
2.11316267860017));
#32738=CARTESIAN_POINT('Ctrl Pts',(-11.2836878397927,-1.55367640539128,
1.48885487031187));
#32739=CARTESIAN_POINT('Ctrl Pts',(-11.17264831978,-2.09393718452755,-0.496010347446261));
#32740=CARTESIAN_POINT('Ctrl Pts',(-11.0616087997673,-0.720699335838131,
-2.02760737443013));
#32741=CARTESIAN_POINT('Ctrl Pts',(-10.9505692797546,1.31113381379501,-1.70631981757357));
#32742=CARTESIAN_POINT('Ctrl Pts',(-10.8395297597419,2.1448160484289,0.174250727180013));
#32743=CARTESIAN_POINT('Ctrl Pts',(-10.7284902397292,1.018505119976,1.89558606190899));
#32744=CARTESIAN_POINT('Ctrl Pts',(-10.6174507197165,-1.03854440173956,
1.88468159728278));
#32745=CARTESIAN_POINT('Ctrl Pts',(-10.5064111997038,-2.14654287151867,
0.15150213943483));
#32746=CARTESIAN_POINT('Ctrl Pts',(-10.3953716796911,-1.29297015875692,
-1.7201242298407));
#32747=CARTESIAN_POINT('Ctrl Pts',(-10.2843321596785,0.742155010727236,
-2.01985275145824));
#32748=CARTESIAN_POINT('Ctrl Pts',(-10.1732926396657,2.09907808076259,-0.473783081571129));
#32749=CARTESIAN_POINT('Ctrl Pts',(-10.0622531196531,1.53780462756055,1.50524287906447));
#32750=CARTESIAN_POINT('Ctrl Pts',(-9.95121359964035,-0.428757898515473,
2.10873560741539));
#32751=CARTESIAN_POINT('Ctrl Pts',(-9.84017407962767,-2.00350941108974,
0.78520649334798));
#32752=CARTESIAN_POINT('Ctrl Pts',(-9.72913455961497,-1.74739773574985,
-1.25586637450696));
#32753=CARTESIAN_POINT('Ctrl Pts',(-9.61809503960229,0.105535083189655,
-2.14929326610798));
#32754=CARTESIAN_POINT('Ctrl Pts',(-9.50705551958959,1.86202697813056,-1.07863558732083));
#32755=CARTESIAN_POINT('Ctrl Pts',(-9.3960159995769,1.91694630730648,0.977709595138056));
#32756=CARTESIAN_POINT('Ctrl Pts',(-9.2849764795642,0.220106244772615,2.14059628107054));
#32757=CARTESIAN_POINT('Ctrl Pts',(-9.17393695955151,-1.67787308806046,
1.34734594588154));
#32758=CARTESIAN_POINT('Ctrl Pts',(-9.06289743953881,-2.04256485362883,
-0.677146967977541));
#32759=CARTESIAN_POINT('Ctrl Pts',(-8.95185791952613,-0.540703470638638,
-2.08284395823602));
#32760=CARTESIAN_POINT('Ctrl Pts',(-8.84081839951343,1.45526793474034,-1.58517962251523));
#32761=CARTESIAN_POINT('Ctrl Pts',(-8.72977887950073,2.12137461599071,0.361066387456933));
#32762=CARTESIAN_POINT('Ctrl Pts',(-8.61873935948805,0.848909573697069,
1.9773597885075));
#32763=CARTESIAN_POINT('Ctrl Pts',(-8.50769983947535,-1.19931288692809,
1.78668626142621));
#32764=CARTESIAN_POINT('Ctrl Pts',(-8.39666031946266,-2.15156953710398,
-0.0367113678183627));
#32765=CARTESIAN_POINT('Ctrl Pts',(-8.28562079944997,-1.13766149650434,
-1.82656111775448));
#32766=CARTESIAN_POINT('Ctrl Pts',(-8.17458127943727,0.915873581896044,
-1.94724800154111));
#32767=CARTESIAN_POINT('Ctrl Pts',(-8.06354175942458,2.13245764993681,-0.28848495410838));
#32768=CARTESIAN_POINT('Ctrl Pts',(-7.95250223941187,1.40034200663875,1.63390374929613));
#32769=CARTESIAN_POINT('Ctrl Pts',(-7.84146271939921,-0.611445504559457,
2.06318530250556));
#32770=CARTESIAN_POINT('Ctrl Pts',(-7.73042319938648,-2.06447693529353,
0.607070161646897));
#32771=CARTESIAN_POINT('Ctrl Pts',(-7.61938367937381,-1.63093134162977,
-1.40380274839831));
#32772=CARTESIAN_POINT('Ctrl Pts',(-7.50834415936112,0.293005132594524,
-2.13184126749489));
#32773=CARTESIAN_POINT('Ctrl Pts',(-7.39730463934841,1.94918528475322,-0.91174334284516));
#32774=CARTESIAN_POINT('Ctrl Pts',(-7.28626511933573,1.82414516186586,1.14153126368152));
#32775=CARTESIAN_POINT('Ctrl Pts',(-7.17522559932303,0.0321499411956851,
2.15164253044089));
#32776=CARTESIAN_POINT('Ctrl Pts',(-7.06418607931035,-1.7892247989831,1.19552240306272));
#32777=CARTESIAN_POINT('Ctrl Pts',(-6.95314655929764,-1.97555565005957,
-0.853099684115907));
#32778=CARTESIAN_POINT('Ctrl Pts',(-6.84210703928496,-0.356568245404698,
-2.12213531234225));
#32779=CARTESIAN_POINT('Ctrl Pts',(-6.73106751927225,1.58826123959035,-1.45190407132699));
#32780=CARTESIAN_POINT('Ctrl Pts',(-6.62002799925957,2.08169298207356,0.545117900922933));
#32781=CARTESIAN_POINT('Ctrl Pts',(-6.50898847924688,0.672815192931128,
2.04399582036804));
#32782=CARTESIAN_POINT('Ctrl Pts',(-6.39794895923417,-1.35090002207445,
1.67501293364566));
#32783=CARTESIAN_POINT('Ctrl Pts',(-6.28690943922149,-2.14012484373404,
-0.224643830881916));
#32784=CARTESIAN_POINT('Ctrl Pts',(-6.17586991920879,-0.973643456955139,
-1.91901475144131));
#32785=CARTESIAN_POINT('Ctrl Pts',(-6.0648303991961,1.08258067504153,-1.85973607792815));
#32786=CARTESIAN_POINT('Ctrl Pts',(-5.95379087918341,2.14951217137112,-0.10097832761718));
#32787=CARTESIAN_POINT('Ctrl Pts',(-5.84275135917072,1.25215905553298,1.75005625542945));
#32788=CARTESIAN_POINT('Ctrl Pts',(-5.73171183915802,-0.789452184324518,
2.00184026490282));
#32789=CARTESIAN_POINT('Ctrl Pts',(-5.62067231914534,-2.10963983869857,
0.424286399141893));
#32790=CARTESIAN_POINT('Ctrl Pts',(-5.50963279913263,-1.50197933870362,
-1.54099229836765));
#32791=CARTESIAN_POINT('Ctrl Pts',(-5.39859327911995,0.478232078705997,
-2.09806893986292));
#32792=CARTESIAN_POINT('Ctrl Pts',(-5.28755375910724,2.02142158679187,-0.737871239426468));
#32793=CARTESIAN_POINT('Ctrl Pts',(-5.17651423909456,1.71737925756923,1.29661392989273));
#32794=CARTESIAN_POINT('Ctrl Pts',(-5.06547471908186,-0.156052486530463,
2.14621686205486));
#32795=CARTESIAN_POINT('Ctrl Pts',(-4.95443519906917,-1.88687908418583,
1.0345465282833));
#32796=CARTESIAN_POINT('Ctrl Pts',(-4.84339567905648,-1.89342256334962,
-1.02252148834121));
#32797=CARTESIAN_POINT('Ctrl Pts',(-4.73235615904378,-0.169703308924683,
-2.14518064145213));
#32798=CARTESIAN_POINT('Ctrl Pts',(-4.62131663903109,1.70909559696464,-1.30751345612848));
#32799=CARTESIAN_POINT('Ctrl Pts',(-4.5102771190184,2.02607492976459,0.724996259645748));
#32800=CARTESIAN_POINT('Ctrl Pts',(-4.39923759900571,0.491570069713157,
2.09498402477993));
#32801=CARTESIAN_POINT('Ctrl Pts',(-4.28819807899301,-1.49214533057168,
1.55051653005515));
#32802=CARTESIAN_POINT('Ctrl Pts',(-4.17715855898032,-2.11229640635658,
-0.41085653118081));
#32803=CARTESIAN_POINT('Ctrl Pts',(-4.06611903896763,-0.802171681611132,
-1.99677735131931));
#32804=CARTESIAN_POINT('Ctrl Pts',(-3.95507951895493,1.24100006258937,-1.7579869288977));
#32805=CARTESIAN_POINT('Ctrl Pts',(-3.84403999894224,2.15011108403084,0.0873013393233009));
#32806=CARTESIAN_POINT('Ctrl Pts',(-3.73300047892955,1.09439019009076,1.85281119096156));
#32807=CARTESIAN_POINT('Ctrl Pts',(-3.62196095891685,-0.961415206155314,
1.92517012206756));
#32808=CARTESIAN_POINT('Ctrl Pts',(-3.51092143890416,-2.13865237631059,
0.238254508484187));
#32809=CARTESIAN_POINT('Ctrl Pts',(-3.39988191889147,-1.36152892013381,
-1.66638476863905));
#32810=CARTESIAN_POINT('Ctrl Pts',(-3.28884239887877,0.659797915063637,
-2.04823482756436));
#32811=CARTESIAN_POINT('Ctrl Pts',(-3.17780287886608,2.07818287860732,-0.558350356417769));
#32812=CARTESIAN_POINT('Ctrl Pts',(-3.06676335885339,1.59746594173181,1.44177035706117));
#32813=CARTESIAN_POINT('Ctrl Pts',(-2.9557238388407,-0.343060253158991,
2.12436081223105));
#32814=CARTESIAN_POINT('Ctrl Pts',(-2.844684318828,-1.97008835036937,0.865650673597296));
#32815=CARTESIAN_POINT('Ctrl Pts',(-2.73364479881531,-1.79679436420783,
-1.18411537033918));
#32816=CARTESIAN_POINT('Ctrl Pts',(-2.62260527880261,0.0184607929944456,
-2.15180352231987));
#32817=CARTESIAN_POINT('Ctrl Pts',(-2.51156575878993,1.81684595782065,-1.1531131596165));
#32818=CARTESIAN_POINT('Ctrl Pts',(-2.40052623877722,1.95494624465731,0.899324401621065));
#32819=CARTESIAN_POINT('Ctrl Pts',(-2.28948671876454,0.30656172550121,2.1299340643318));
#32820=CARTESIAN_POINT('Ctrl Pts',(-2.17844719875184,-1.6219675037033,1.41415012780357));
#32821=CARTESIAN_POINT('Ctrl Pts',(-2.06740767873915,-2.06829727352021,
-0.593923904133282));
#32822=CARTESIAN_POINT('Ctrl Pts',(-1.95636815872646,-0.624558859445587,
-2.05925362733538));
#32823=CARTESIAN_POINT('Ctrl Pts',(-1.84532863871376,1.38991893566234,-1.64277945370315));
#32824=CARTESIAN_POINT('Ctrl Pts',(-1.73428911870107,2.13424985602369,0.274912589779238));
#32825=CARTESIAN_POINT('Ctrl Pts',(-1.62324959868838,0.928243110203279,
1.94138206745225));
#32826=CARTESIAN_POINT('Ctrl Pts',(-1.51221007867568,-1.12601791350259,
1.83376153213378));
#32827=CARTESIAN_POINT('Ctrl Pts',(-1.40117055866299,-2.15129280801212,
0.0503992116640912));
#32828=CARTESIAN_POINT('Ctrl Pts',(-1.2901310386503,-1.21065460969833,-1.7790212687057));
#32829=CARTESIAN_POINT('Ctrl Pts',(-1.17909151863761,0.836311339433325,
-1.98271843339464));
#32830=CARTESIAN_POINT('Ctrl Pts',(-1.06805199862491,2.11903714154564,-0.374558827692656));
#32831=CARTESIAN_POINT('Ctrl Pts',(-0.95701247861222,1.46531842129889,1.57589654811268));
#32832=CARTESIAN_POINT('Ctrl Pts',(-0.845972958599524,-0.527432604959965,
2.08622790808164));
#32833=CARTESIAN_POINT('Ctrl Pts',(-0.734933438586833,-2.03823292861889,
0.690154063009435));
#32834=CARTESIAN_POINT('Ctrl Pts',(-0.623893918574141,-1.68637779932512,
-1.33669417120906));
#32835=CARTESIAN_POINT('Ctrl Pts',(-0.512854398561449,0.206420798547222,
-2.14185826474789));
#32836=CARTESIAN_POINT('Ctrl Pts',(-0.401814878548749,1.91080687781125,
-0.990065952857435));
#32837=CARTESIAN_POINT('Ctrl Pts',(-0.290775358536063,1.86862407709947,
1.06711197204293));
#32838=CARTESIAN_POINT('Ctrl Pts',(-0.179735838523365,0.119640249212883,
2.14792080547069));
#32839=CARTESIAN_POINT('Ctrl Pts',(-0.0686963185106752,-1.74020790821638,
1.26823181386572));
#32840=CARTESIAN_POINT('Ctrl Pts',(0.0423432015020179,-2.0067891538205,
-0.775065728985946));
#32841=CARTESIAN_POINT('Ctrl Pts',(0.116369548177145,-0.966344453583496,
-1.65798255609091));
#32842=CARTESIAN_POINT('Ctrl Pts',(0.15338272151471,-0.374209849651479,
-1.78230609497965));
#32843=CARTESIAN_POINT('Ctrl Pts',(-19.646,-0.861525859670562,1.75382131162753));
#32844=CARTESIAN_POINT('Ctrl Pts',(-19.6089868266624,-1.44419697921243,
1.46759703447886));
#32845=CARTESIAN_POINT('Ctrl Pts',(-19.5349604799873,-2.29187071398093,
0.273839964503935));
#32846=CARTESIAN_POINT('Ctrl Pts',(-19.4239209599746,-1.47305782540113,
-1.77985889120705));
#32847=CARTESIAN_POINT('Ctrl Pts',(-19.3128814399619,0.693776360936581,
-2.20142548720342));
#32848=CARTESIAN_POINT('Ctrl Pts',(-19.2018419199492,2.22564199091573,-0.614099290755457));
#32849=CARTESIAN_POINT('Ctrl Pts',(-19.0908023999365,1.72416400219814,1.53588048752263));
#32850=CARTESIAN_POINT('Ctrl Pts',(-18.9797628799238,-0.353171550044496,
2.28155747838165));
#32851=CARTESIAN_POINT('Ctrl Pts',(-18.8687233599112,-2.10762815878697,
0.942688723589834));
#32852=CARTESIAN_POINT('Ctrl Pts',(-18.7576838398985,-1.93614897507197,
-1.25784862067171));
#32853=CARTESIAN_POINT('Ctrl Pts',(-18.6466443198858,0.00467644902946805,
-2.30881652674107));
#32854=CARTESIAN_POINT('Ctrl Pts',(-18.5356047998731,1.9412079506099,-1.24998190827883));
#32855=CARTESIAN_POINT('Ctrl Pts',(-18.4245652798604,2.10381983890809,0.951152245213705));
#32856=CARTESIAN_POINT('Ctrl Pts',(-18.3135257598477,0.343896402045778,
2.28308048749787));
#32857=CARTESIAN_POINT('Ctrl Pts',(-18.202486239835,-1.73028625894889,1.52867418789625));
#32858=CARTESIAN_POINT('Ctrl Pts',(-18.0914467198223,-2.2232862854983,-0.622682026296723));
#32859=CARTESIAN_POINT('Ctrl Pts',(-17.9804071998096,-0.684584021301682,
-2.20501154870007));
#32860=CARTESIAN_POINT('Ctrl Pts',(-17.8693676797969,1.4797099235446,-1.77234081021396));
#32861=CARTESIAN_POINT('Ctrl Pts',(-17.7583281597842,2.29180359485407,0.279945406637725));
#32862=CARTESIAN_POINT('Ctrl Pts',(-17.6472886397715,1.0095826344478,2.07640930292734));
#32863=CARTESIAN_POINT('Ctrl Pts',(-17.5362491197588,-1.19522323865519,
1.97539222231392));
#32864=CARTESIAN_POINT('Ctrl Pts',(-17.4252095997461,-2.30780056970933,
0.0692061360807777));
#32865=CARTESIAN_POINT('Ctrl Pts',(-17.3141700797335,-1.31144488582588,
-1.90022241182763));
#32866=CARTESIAN_POINT('Ctrl Pts',(-17.2031305597207,0.883345970326033,
-2.13317435974508));
#32867=CARTESIAN_POINT('Ctrl Pts',(-17.0920910397081,2.2709104662044,-0.416771633006387));
#32868=CARTESIAN_POINT('Ctrl Pts',(-16.9810515196954,1.58325317493202,1.68048871382927));
#32869=CARTESIAN_POINT('Ctrl Pts',(-16.8700119996827,-0.55122534734696,
2.2420712648884));
#32870=CARTESIAN_POINT('Ctrl Pts',(-16.75897247967,-2.18197866138569,0.754786101702939));
#32871=CARTESIAN_POINT('Ctrl Pts',(-16.6479329596573,-1.81877857217932,
-1.42224380568198));
#32872=CARTESIAN_POINT('Ctrl Pts',(-16.5368934396446,0.206472474189701,
-2.2995873664278));
#32873=CARTESIAN_POINT('Ctrl Pts',(-16.4258539196319,2.04304317295608,-1.0755033851506));
#32874=CARTESIAN_POINT('Ctrl Pts',(-16.3148143996192,2.01262362147143,1.13140580530432));
#32875=CARTESIAN_POINT('Ctrl Pts',(-16.2037748796065,0.143012060592391,
2.3044045844092));
#32876=CARTESIAN_POINT('Ctrl Pts',(-16.0927353595938,-1.85728793915615,
1.37157371260918));
#32877=CARTESIAN_POINT('Ctrl Pts',(-15.9816958395811,-2.16034604008886,
-0.814639751747095));
#32878=CARTESIAN_POINT('Ctrl Pts',(-15.8706563195684,-0.489219235248991,
-2.25641252388286));
#32879=CARTESIAN_POINT('Ctrl Pts',(-15.7596167995557,1.62896985124693,-1.63621213838278));
#32880=CARTESIAN_POINT('Ctrl Pts',(-15.648577279543,2.25856052220058,0.479204868110092));
#32881=CARTESIAN_POINT('Ctrl Pts',(-15.5375377595304,0.82421513431492,2.15671100299323));
#32882=CARTESIAN_POINT('Ctrl Pts',(-15.4264982395177,-1.36332119941149,
1.86335403112222));
#32883=CARTESIAN_POINT('Ctrl Pts',(-15.315458719505,-2.30501631897153,-0.132788204820276));
#32884=CARTESIAN_POINT('Ctrl Pts',(-15.2044191994923,-1.1403227674393,-2.00758484854921));
#32885=CARTESIAN_POINT('Ctrl Pts',(-15.0933796794796,1.06642976604176,-2.04779405511507));
#32886=CARTESIAN_POINT('Ctrl Pts',(-14.9823401594669,2.29864881825516,-0.216671521891302));
#32887=CARTESIAN_POINT('Ctrl Pts',(-14.8713006394542,1.43029800042407,1.81245153536515));
#32888=CARTESIAN_POINT('Ctrl Pts',(-14.7602611194415,-0.74509931403381,
2.18530545926443));
#32889=CARTESIAN_POINT('Ctrl Pts',(-14.6492215994288,-2.23960394196192,
0.561165858916255));
#32890=CARTESIAN_POINT('Ctrl Pts',(-14.5381820794161,-1.68749556665226,
-1.57578286911412));
#32891=CARTESIAN_POINT('Ctrl Pts',(-14.4271425594034,0.406693667200237,
-2.27273694015031));
#32892=CARTESIAN_POINT('Ctrl Pts',(-14.3161030393907,2.12923480201551,-0.892800143341485));
#32893=CARTESIAN_POINT('Ctrl Pts',(-14.205063519378,1.90602135446747,1.30300250743372));
#32894=CARTESIAN_POINT('Ctrl Pts',(-14.0940239993654,-0.0589679559524329,
2.3080848594095));
#32895=CARTESIAN_POINT('Ctrl Pts',(-13.9829844793526,-1.97007069153408,
1.20397442183089));
#32896=CARTESIAN_POINT('Ctrl Pts',(-13.87194495934,-2.08086748058341,-1.00036166775573));
#32897=CARTESIAN_POINT('Ctrl Pts',(-13.7609054393273,-0.290109104461037,
-2.29053916045402));
#32898=CARTESIAN_POINT('Ctrl Pts',(-13.6498659193146,1.76575912185542,-1.48755761624515));
#32899=CARTESIAN_POINT('Ctrl Pts',(-13.5388263993019,2.20802705409076,0.674795870221375));
#32900=CARTESIAN_POINT('Ctrl Pts',(-13.4277868792892,0.632537830369223,
2.22050193227036));
#32901=CARTESIAN_POINT('Ctrl Pts',(-13.3167473592765,-1.52098223372466,
1.73705094420357));
#32902=CARTESIAN_POINT('Ctrl Pts',(-13.2057078392638,-2.28458600105243,
-0.333765998657508));
#32903=CARTESIAN_POINT('Ctrl Pts',(-13.0946683192511,-0.960470895786627,
-2.09957819487902));
#32904=CARTESIAN_POINT('Ctrl Pts',(-12.9836287992384,1.24134949822159,-1.94673684953298));
#32905=CARTESIAN_POINT('Ctrl Pts',(-12.8725892792257,2.30878984537321,-0.0149126780332815));
#32906=CARTESIAN_POINT('Ctrl Pts',(-12.761549759213,1.26639316699041,1.93053911762093));
#32907=CARTESIAN_POINT('Ctrl Pts',(-12.6505102392003,-0.933269166365103,
2.11181002961364));
#32908=CARTESIAN_POINT('Ctrl Pts',(-12.5394707191876,-2.28008391554889,
0.363249605808196));
#32909=CARTESIAN_POINT('Ctrl Pts',(-12.428431199175,-1.54329392435714,-1.71725851318516));
#32910=CARTESIAN_POINT('Ctrl Pts',(-12.3173916791623,0.603801413341659,
-2.2284875569119));
#32911=CARTESIAN_POINT('Ctrl Pts',(-12.2063521591496,2.19912605588985,-0.703262062371451));
#32912=CARTESIAN_POINT('Ctrl Pts',(-12.0953126391369,1.7848275247083,1.46462406272333));
#32913=CARTESIAN_POINT('Ctrl Pts',(-11.9842731191242,-0.260496542802998,
2.29409557108074));
#32914=CARTESIAN_POINT('Ctrl Pts',(-11.8732335991115,-2.0677715509203,1.02715809458389));
#32915=CARTESIAN_POINT('Ctrl Pts',(-11.7621940790988,-1.9854588223187,-1.1784253064753));
#32916=CARTESIAN_POINT('Ctrl Pts',(-11.6511545590861,-0.0887780409483811,
-2.30713055493398));
#32917=CARTESIAN_POINT('Ctrl Pts',(-11.5401150390734,1.88903060843585,-1.32751508407891));
#32918=CARTESIAN_POINT('Ctrl Pts',(-11.4290755190607,2.14059001602237,0.865220966788218));
#32919=CARTESIAN_POINT('Ctrl Pts',(-11.318035999048,0.436018127664415,2.26729379005294));
#32920=CARTESIAN_POINT('Ctrl Pts',(-11.2069964790353,-1.6669993755658,1.59744984895545));
#32921=CARTESIAN_POINT('Ctrl Pts',(-11.0959569590226,-2.24666601550298,
-0.53218864404321));
#32922=CARTESIAN_POINT('Ctrl Pts',(-10.9849174390099,-0.773266130993508,
-2.17549820241776));
#32923=CARTESIAN_POINT('Ctrl Pts',(-10.8738779189972,1.40676606872269,-1.83077638338358));
#32924=CARTESIAN_POINT('Ctrl Pts',(-10.7628383989846,2.30125591212414,0.186960329958694));
#32925=CARTESIAN_POINT('Ctrl Pts',(-10.6517988789719,1.09279344985801,2.03384744118433));
#32926=CARTESIAN_POINT('Ctrl Pts',(-10.5407593589592,-1.11429436862769,
2.02214762025654));
#32927=CARTESIAN_POINT('Ctrl Pts',(-10.4297198389465,-2.30310868725953,
0.162552492242497));
#32928=CARTESIAN_POINT('Ctrl Pts',(-10.3186803189338,-1.38727758225186,
-1.84558767005147));
#32929=CARTESIAN_POINT('Ctrl Pts',(-10.2076407989211,0.796286752609709,
-2.1671779681611));
#32930=CARTESIAN_POINT('Ctrl Pts',(-10.0966012789084,2.25218188147347,-0.508340152680491));
#32931=CARTESIAN_POINT('Ctrl Pts',(-9.9855617588957,1.64996993259997,1.615033176));
#32932=CARTESIAN_POINT('Ctrl Pts',(-9.87452223888301,-0.460030896146754,
2.26254381452713));
#32933=CARTESIAN_POINT('Ctrl Pts',(-9.7634827188703,-2.14964256754975,0.842478349776842));
#32934=CARTESIAN_POINT('Ctrl Pts',(-9.65244319885763,-1.87485046709354,
-1.34746750020314));
#32935=CARTESIAN_POINT('Ctrl Pts',(-9.54140367884492,0.113232663614504,
-2.30605969175894));
#32936=CARTESIAN_POINT('Ctrl Pts',(-9.43036415883224,1.99784060507026,-1.15730974885597));
#32937=CARTESIAN_POINT('Ctrl Pts',(-9.31932463881954,2.05676567281605,1.04902235685904));
#32938=CARTESIAN_POINT('Ctrl Pts',(-9.20828511880685,0.23616048446179,2.29672836087408));
#32939=CARTESIAN_POINT('Ctrl Pts',(-9.09724559879414,-1.80025478945923,
1.44561946275418));
#32940=CARTESIAN_POINT('Ctrl Pts',(-8.98620607878147,-2.19154665909622,
-0.726537114722142));
#32941=CARTESIAN_POINT('Ctrl Pts',(-8.87516655876876,-0.580141620734622,
-2.23476366489971));
#32942=CARTESIAN_POINT('Ctrl Pts',(-8.76412703875608,1.56141312957773,-1.70080039300526));
#32943=CARTESIAN_POINT('Ctrl Pts',(-8.65308751874337,2.27610469459825,0.387402061548938));
#32944=CARTESIAN_POINT('Ctrl Pts',(-8.54204799873069,0.910827843143066,
2.12158562830256));
#32945=CARTESIAN_POINT('Ctrl Pts',(-8.431008478718,-1.28678908084058,1.91700464253325));
#32946=CARTESIAN_POINT('Ctrl Pts',(-8.3199689587053,-2.30850199075749,-0.0393890433149694));
#32947=CARTESIAN_POINT('Ctrl Pts',(-8.20892943869261,-1.22064092477503,
-1.95978791475735));
#32948=CARTESIAN_POINT('Ctrl Pts',(-8.09788991867992,0.982676111846747,
-2.08927752997785));
#32949=CARTESIAN_POINT('Ctrl Pts',(-7.98685039866722,2.28799610944076,-0.309526640611922));
#32950=CARTESIAN_POINT('Ctrl Pts',(-7.87581087865452,1.50248098158987,1.75307838901326));
#32951=CARTESIAN_POINT('Ctrl Pts',(-7.76477135864184,-0.656043479038643,
2.21367113449027));
#32952=CARTESIAN_POINT('Ctrl Pts',(-7.65373183862914,-2.2150569771558,0.651349004772403));
#32953=CARTESIAN_POINT('Ctrl Pts',(-7.54269231861645,-1.74988917811544,
-1.50619414498233));
#32954=CARTESIAN_POINT('Ctrl Pts',(-7.43165279860375,0.314376514554623,
-2.2873347689311));
#32955=CARTESIAN_POINT('Ctrl Pts',(-7.32061327859107,2.09135611590069,-0.978244618972865));
#32956=CARTESIAN_POINT('Ctrl Pts',(-7.20957375857837,1.95719574244671,1.22479294732335));
#32957=CARTESIAN_POINT('Ctrl Pts',(-7.09853423856569,0.0344949126547129,
2.30858030812565));
#32958=CARTESIAN_POINT('Ctrl Pts',(-6.98749471855298,-1.91972833744651,
1.28272212441724));
#32959=CARTESIAN_POINT('Ctrl Pts',(-6.87645519854029,-2.11964989853558,
-0.915323574318207));
#32960=CARTESIAN_POINT('Ctrl Pts',(-6.76541567852761,-0.382575831346619,
-2.27692087507098));
#32961=CARTESIAN_POINT('Ctrl Pts',(-6.65437615851489,1.70410677889241,-1.5578039107017));
#32962=CARTESIAN_POINT('Ctrl Pts',(-6.54333663850222,2.23352873815598,0.584878033350475));
#32963=CARTESIAN_POINT('Ctrl Pts',(-6.43229711848952,0.721889386100885,
2.19308199853527));
#32964=CARTESIAN_POINT('Ctrl Pts',(-6.32125759847682,-1.44943276826219,
1.79718601940713));
#32965=CARTESIAN_POINT('Ctrl Pts',(-6.21021807846414,-2.29622253756181,
-0.241029035715179));
#32966=CARTESIAN_POINT('Ctrl Pts',(-6.09917855845143,-1.04465964028021,
-2.05898498635472));
#32967=CARTESIAN_POINT('Ctrl Pts',(-5.98813903843876,1.16154258572225,-1.99538260983157));
#32968=CARTESIAN_POINT('Ctrl Pts',(-5.87709951842604,2.30629456366387,-0.108343544704277));
#32969=CARTESIAN_POINT('Ctrl Pts',(-5.76605999841337,1.34348977460131,1.87770289545666));
#32970=CARTESIAN_POINT('Ctrl Pts',(-5.65502047840067,-0.847033715477332,
2.14785167618931));
#32971=CARTESIAN_POINT('Ctrl Pts',(-5.54398095838797,-2.26351399916739,
0.455233251902571));
#32972=CARTESIAN_POINT('Ctrl Pts',(-5.43294143837529,-1.61153159759871,
-1.65339010762904));
#32973=CARTESIAN_POINT('Ctrl Pts',(-5.32190191836258,0.513113653404346,
-2.25109913525696));
#32974=CARTESIAN_POINT('Ctrl Pts',(-5.2108623983499,2.16886123213581,-0.791690529059738));
#32975=CARTESIAN_POINT('Ctrl Pts',(-5.0998228783372,1.84264248336612,1.39118712492565));
#32976=CARTESIAN_POINT('Ctrl Pts',(-4.98878335832451,-0.167434735250603,
2.3027588991243));
#32977=CARTESIAN_POINT('Ctrl Pts',(-4.87774383831182,-2.0245053887613,1.1100048959086));
#32978=CARTESIAN_POINT('Ctrl Pts',(-4.76670431829912,-2.03152614008519,
-1.09710276647867));
#32979=CARTESIAN_POINT('Ctrl Pts',(-4.65566479828643,-0.182081229416383,
-2.30164709804931));
#32980=CARTESIAN_POINT('Ctrl Pts',(-4.54462527827374,1.83375462421648,-1.40288164726367));
#32981=CARTESIAN_POINT('Ctrl Pts',(-4.43358575826104,2.17385398339526,0.777876466375666));
#32982=CARTESIAN_POINT('Ctrl Pts',(-4.32254623824835,0.527424498702014,
2.24778921080992));
#32983=CARTESIAN_POINT('Ctrl Pts',(-4.21150671823566,-1.60098031075524,
1.66360902337022));
#32984=CARTESIAN_POINT('Ctrl Pts',(-4.10046719822296,-2.26636433313119,
-0.44082382827528));
#32985=CARTESIAN_POINT('Ctrl Pts',(-3.98942767821027,-0.860680954993021,
-2.1424194808152));
#32986=CARTESIAN_POINT('Ctrl Pts',(-3.87838815819758,1.33151686041895,-1.88621202108507));
#32987=CARTESIAN_POINT('Ctrl Pts',(-3.76734863818489,2.30693716017,0.093668976134945));
#32988=CARTESIAN_POINT('Ctrl Pts',(-3.65630911817219,1.17421347017698,1.98795263135658));
#32989=CARTESIAN_POINT('Ctrl Pts',(-3.5452695981595,-1.03153947807862,2.06558932105061));
#32990=CARTESIAN_POINT('Ctrl Pts',(-3.4342300781468,-2.29464267043703,0.255632456984391));
#32991=CARTESIAN_POINT('Ctrl Pts',(-3.32319055813411,-1.46083692318556,
-1.78792852818929));
#32992=CARTESIAN_POINT('Ctrl Pts',(-3.21215103812142,0.707922646307885,
-2.19763019294999));
#32993=CARTESIAN_POINT('Ctrl Pts',(-3.10111151810873,2.22976261268347,-0.599075645524091));
#32994=CARTESIAN_POINT('Ctrl Pts',(-2.99007199809603,1.71398285905222,1.54693105758079));
#32995=CARTESIAN_POINT('Ctrl Pts',(-2.87903247808334,-0.36808258515935,
2.27930869978922));
#32996=CARTESIAN_POINT('Ctrl Pts',(-2.76799295807064,-2.11378382170134,
0.928790015306536));
#32997=CARTESIAN_POINT('Ctrl Pts',(-2.65695343805796,-1.92785001610438,
-1.27048307878253));
#32998=CARTESIAN_POINT('Ctrl Pts',(-2.54591391804526,0.0198072972514943,
-2.30875304252568));
#32999=CARTESIAN_POINT('Ctrl Pts',(-2.43487439803257,1.94936414473225,-1.23721961044602));
#33000=CARTESIAN_POINT('Ctrl Pts',(-2.32383487801987,2.09753727211149,0.964919857655855));
#33001=CARTESIAN_POINT('Ctrl Pts',(-2.21279535800718,0.328921906266679,
2.28528845705372));
#33002=CARTESIAN_POINT('Ctrl Pts',(-2.10175583799449,-1.74027153046743,
1.51729624767722));
#33003=CARTESIAN_POINT('Ctrl Pts',(-1.9907163179818,-2.21915596547551,-0.637243877739432));
#33004=CARTESIAN_POINT('Ctrl Pts',(-1.8796767979691,-0.670113303572792,
-2.2094526884671));
#33005=CARTESIAN_POINT('Ctrl Pts',(-1.76863727795641,1.49129766648718,-1.76260147480695));
#33006=CARTESIAN_POINT('Ctrl Pts',(-1.65759775794372,2.28991903651704,0.294964327132055));
#33007=CARTESIAN_POINT('Ctrl Pts',(-1.54655823793102,0.995947856138289,
2.08298374291299));
#33008=CARTESIAN_POINT('Ctrl Pts',(-1.43551871791833,-1.20814807521776,
1.96751351722672));
#33009=CARTESIAN_POINT('Ctrl Pts',(-1.32447919790564,-2.30820507743518,
0.0540752592248201));
#33010=CARTESIAN_POINT('Ctrl Pts',(-1.21343967789294,-1.29895805290592,
-1.90878057603237));
#33011=CARTESIAN_POINT('Ctrl Pts',(-1.10240015788025,0.897310711404452,
-2.12733512520534));
#33012=CARTESIAN_POINT('Ctrl Pts',(-0.991360637867558,2.27359672805721,
-0.401878621384507));
#33013=CARTESIAN_POINT('Ctrl Pts',(-0.880321117854865,1.57219668447955,
1.69084022422195));
#33014=CARTESIAN_POINT('Ctrl Pts',(-0.769281597842169,-0.565902796792421,
2.23839443528408));
#33015=CARTESIAN_POINT('Ctrl Pts',(-0.658242077829478,-2.18689876957334,
0.740492928957852));
#33016=CARTESIAN_POINT('Ctrl Pts',(-0.547202557816786,-1.80937982239294,
-1.43419076262974));
#33017=CARTESIAN_POINT('Ctrl Pts',(-0.436163037804094,0.221476841051321,
-2.29808239186457));
#33018=CARTESIAN_POINT('Ctrl Pts',(-0.325123517791394,2.05017844197486,
-1.06227996991859));
#33019=CARTESIAN_POINT('Ctrl Pts',(-0.214083997778708,2.00491888715238,
1.14494561729948));
#33020=CARTESIAN_POINT('Ctrl Pts',(-0.10304447776601,0.128366640594097,
2.30458712577454));
#33021=CARTESIAN_POINT('Ctrl Pts',(0.00799504224667972,-1.86713622365964,
1.36073485730407));
#33022=CARTESIAN_POINT('Ctrl Pts',(0.119034562259373,-2.15316153009897,
-0.831597932335627));
#33023=CARTESIAN_POINT('Ctrl Pts',(0.1930609089345,-1.03682825787616,-1.77891347008418));
#33024=CARTESIAN_POINT('Ctrl Pts',(0.230074082272065,-0.401504189376206,
-1.91230499291127));
#33025=CARTESIAN_POINT('',(-3.47334515779567E-15,-1.49576112924109,1.26226672651054));
#33026=CARTESIAN_POINT('Ctrl Pts',(1.30451205393456E-15,-1.49576882860604,
1.26227079838504));
#33027=CARTESIAN_POINT('Ctrl Pts',(1.26307732327094E-15,-1.52238887744143,
1.22395926652586));
#33028=CARTESIAN_POINT('Ctrl Pts',(5.84589016432815E-15,-1.54749918699467,
1.18468636375502));
#33029=CARTESIAN_POINT('Ctrl Pts',(6.21724893790088E-15,-1.57101022548392,
1.14448601145151));
#33030=CARTESIAN_POINT('Ctrl Pts',(6.79018338235568E-15,-1.60728319042775,
1.08246467749374));
#33031=CARTESIAN_POINT('Ctrl Pts',(9.85209575142001E-15,-1.63975192740418,
1.01823590395021));
#33032=CARTESIAN_POINT('Ctrl Pts',(1.33504318711175E-14,-1.66840521532328,
0.952176670234068));
#33033=CARTESIAN_POINT('Ctrl Pts',(1.5040522558895E-14,-1.68224798326476,
0.920262613972653));
#33034=CARTESIAN_POINT('Ctrl Pts',(2.12362379568834E-16,-1.69519946625923,
0.887921168479435));
#33035=CARTESIAN_POINT('Ctrl Pts',(-2.77555756156289E-17,-1.70725413156156,
0.85519453645218));
#33036=CARTESIAN_POINT('Ctrl Pts',(-1.29001408656712E-16,-1.71233698606792,
0.841395338804994));
#33037=CARTESIAN_POINT('Ctrl Pts',(4.27514254701297E-15,-1.71726036257382,
0.827527661185538));
#33038=CARTESIAN_POINT('Ctrl Pts',(3.94129173741931E-15,-1.72202369968651,
0.813594684328385));
#33039=CARTESIAN_POINT('Ctrl Pts',(3.62096552284113E-15,-1.72659406975068,
0.800226144830491));
#33040=CARTESIAN_POINT('Ctrl Pts',(2.32644902118985E-15,-1.73101538799027,
0.786802333572161));
#33041=CARTESIAN_POINT('Ctrl Pts',(2.63677968348475E-15,-1.73528526710846,
0.773333511905552));
#33042=CARTESIAN_POINT('Ctrl Pts',(4.20467166006644E-15,-1.75685809256139,
0.705284620864877));
#33043=CARTESIAN_POINT('Ctrl Pts',(1.47365000165689E-15,-1.77458920356206,
0.636029775253738));
#33044=CARTESIAN_POINT('Ctrl Pts',(1.36002320516582E-15,-1.78846506651383,
0.565940828545306));
#33045=CARTESIAN_POINT('Ctrl Pts',(1.27834854242507E-15,-1.79843900278432,
0.51556106548726));
#33046=CARTESIAN_POINT('Ctrl Pts',(6.37284015678416E-15,-1.80641993884282,
0.46475008199631));
#33047=CARTESIAN_POINT('Ctrl Pts',(6.07847105982273E-15,-1.81238629657331,
0.413647700170702));
#33048=CARTESIAN_POINT('Ctrl Pts',(5.9169951520491E-15,-1.81565913682923,
0.385615533819469));
#33049=CARTESIAN_POINT('Ctrl Pts',(3.8882620403915E-15,-1.81832553753825,
0.357495735434968));
#33050=CARTESIAN_POINT('Ctrl Pts',(4.413136522885E-15,-1.82038020010595,
0.329311981061615));
#33051=CARTESIAN_POINT('Ctrl Pts',(4.64123187199515E-15,-1.82127309734388,
0.317064132275969));
#33052=CARTESIAN_POINT('Ctrl Pts',(-3.94730007868664E-15,-1.82205028923469,
0.304805345141405));
#33053=CARTESIAN_POINT('Ctrl Pts',(-3.88578058618805E-15,-1.82271089774678,
0.292550090914232));
#33054=CARTESIAN_POINT('Ctrl Pts',(-3.53663723185213E-15,-1.82646006833395,
0.222997492293347));
#33055=CARTESIAN_POINT('Ctrl Pts',(-9.71519400458447E-16,-1.82646676303548,
0.153449623029913));
#33056=CARTESIAN_POINT('Ctrl Pts',(-4.9960036108132E-16,-1.82271640812221,
0.0842505500111845));
#33057=CARTESIAN_POINT('Ctrl Pts',(-3.8896594232137E-17,-1.81905518131974,
0.0166960100539114));
#33058=CARTESIAN_POINT('Ctrl Pts',(-2.20143127797879E-15,-1.81181305450115,
-0.0505270526769876));
#33059=CARTESIAN_POINT('Ctrl Pts',(-3.63598040564739E-15,-1.80092992405888,
-0.117084349296312));
#33060=CARTESIAN_POINT('Ctrl Pts',(-4.59707087045625E-15,-1.79363866250945,
-0.161675072549023));
#33061=CARTESIAN_POINT('Ctrl Pts',(-7.24725434000752E-15,-1.78471220461912,
-0.205966658589872));
#33062=CARTESIAN_POINT('Ctrl Pts',(-7.79931674799172E-15,-1.7741212964033,
-0.249851830349142));
#33063=CARTESIAN_POINT('Ctrl Pts',(-8.24041846233515E-15,-1.76565908687249,
-0.284916388662309));
#33064=CARTESIAN_POINT('Ctrl Pts',(5.28590280211643E-16,-1.75613409737704,
-0.31972140139832));
#33065=CARTESIAN_POINT('Ctrl Pts',(6.66133814775094E-16,-1.74552739422258,
-0.354208724051798));
#33066=CARTESIAN_POINT('Ctrl Pts',(7.24534204826618E-16,-1.74102383392549,
-0.368851892130823));
#33067=CARTESIAN_POINT('Ctrl Pts',(-7.28293105322084E-16,-1.73632360239176,
-0.383442108934698));
#33068=CARTESIAN_POINT('Ctrl Pts',(-8.04911692853238E-16,-1.731434767294,
-0.397947207271473));
#33069=CARTESIAN_POINT('Ctrl Pts',(-1.13106292697556E-15,-1.7106238955208,
-0.459692742865968));
#33070=CARTESIAN_POINT('Ctrl Pts',(4.18317703168387E-15,-1.68637376486003,
-0.519987462298931));
#33071=CARTESIAN_POINT('Ctrl Pts',(3.1641356201817E-15,-1.65863595149533,
-0.578525678013812));
#33072=CARTESIAN_POINT('Ctrl Pts',(2.86946734591812E-15,-1.65061522387449,
-0.595452718277804));
#33073=CARTESIAN_POINT('Ctrl Pts',(5.57580897614692E-15,-1.64230259171472,
-0.612232718698034));
#33074=CARTESIAN_POINT('Ctrl Pts',(5.41233724504764E-15,-1.63369620203523,
-0.628857825595402));
#33075=CARTESIAN_POINT('Ctrl Pts',(4.79851125833417E-15,-1.6021508290194,
-0.68979455028902));
#33076=CARTESIAN_POINT('Ctrl Pts',(-3.78633153299722E-15,-1.56666180412204,
-0.748653919227771));
#33077=CARTESIAN_POINT('Ctrl Pts',(-3.78863607153335E-15,-1.52754044393195,
-0.805204911162976));
#33078=CARTESIAN_POINT('Ctrl Pts',(-3.79072214767112E-15,-1.49212765534529,
-0.856395061813092));
#33079=CARTESIAN_POINT('Ctrl Pts',(-2.05473902985757E-16,-1.45373734054848,
-0.90569356900811));
#33080=CARTESIAN_POINT('Ctrl Pts',(8.18789480661053E-16,-1.4125803735405,
-0.952892246296203));
#33081=CARTESIAN_POINT('Ctrl Pts',(1.01336693800835E-15,-1.40476185916187,
-0.961858493419257));
#33082=CARTESIAN_POINT('Ctrl Pts',(-1.57502819886435E-15,-1.39684930901895,
-0.970742099247602));
#33083=CARTESIAN_POINT('Ctrl Pts',(-1.51267887105178E-15,-1.38884786051959,
-0.97953835419035));
#33084=CARTESIAN_POINT('Ctrl Pts',(-1.1728207214089E-15,-1.34523299606383,
-1.0274856061257));
#33085=CARTESIAN_POINT('Ctrl Pts',(4.26408912821895E-15,-1.29894819098313,
-1.07287671206358));
#33086=CARTESIAN_POINT('Ctrl Pts',(3.09474668114262E-15,-1.25027379293301,
-1.11553472901405));
#33087=CARTESIAN_POINT('Ctrl Pts',(1.9305259728076E-15,-1.20181258952987,
-1.1580059031636));
#33088=CARTESIAN_POINT('Ctrl Pts',(-1.33080683399921E-15,-1.1509816522108,
-1.19776833545068));
#33089=CARTESIAN_POINT('Ctrl Pts',(-1.31145094783847E-15,-1.09803478904449,
-1.23460162248222));
#33090=CARTESIAN_POINT('Ctrl Pts',(-1.29249638855516E-15,-1.0461857314288,
-1.27067120446058));
#33091=CARTESIAN_POINT('Ctrl Pts',(5.22726634415042E-16,-0.992306651654647,
-1.3039321130855));
#33092=CARTESIAN_POINT('Ctrl Pts',(1.40165656858926E-15,-0.936628381019438,
-1.33412827396106));
#33093=CARTESIAN_POINT('Ctrl Pts',(1.55885413648105E-15,-0.92667026218884,
-1.33952888994277));
#33094=CARTESIAN_POINT('Ctrl Pts',(6.8101243531962E-15,-0.916654592115581,
-1.344831336662));
#33095=CARTESIAN_POINT('Ctrl Pts',(7.13318293321663E-15,-0.906582699777643,
-1.35003396913283));
#33096=CARTESIAN_POINT('Ctrl Pts',(7.43361135889431E-15,-0.897216340405636,
-1.35487215879643));
#33097=CARTESIAN_POINT('Ctrl Pts',(2.40141014764684E-15,-0.887809725328665,
-1.35961970024266));
#33098=CARTESIAN_POINT('Ctrl Pts',(2.23432383705813E-15,-0.878364903116739,
-1.36427535802199));
#33099=CARTESIAN_POINT('Ctrl Pts',(1.25007779416339E-15,-0.822728813869338,
-1.39170018253469));
#33100=CARTESIAN_POINT('Ctrl Pts',(7.66888170002638E-16,-0.765757994888109,
-1.41594579927101));
#33101=CARTESIAN_POINT('Ctrl Pts',(-7.97972798949331E-17,-0.707686469549987,
-1.43682247825627));
#33102=CARTESIAN_POINT('Ctrl Pts',(-9.11162927195913E-16,-0.650665681891094,
-1.4573214176678));
#33103=CARTESIAN_POINT('Ctrl Pts',(-2.79461917356239E-15,-0.59258279903694,
-1.47457243551005));
#33104=CARTESIAN_POINT('Ctrl Pts',(-3.42607886505419E-15,-0.533655823086145,
-1.48834629363144));
#33105=CARTESIAN_POINT('Ctrl Pts',(-4.03744356266809E-15,-0.476604085154388,
-1.50168182512904));
#33106=CARTESIAN_POINT('Ctrl Pts',(2.17949943466874E-15,-0.4187604494125,
-1.51175801196898));
#33107=CARTESIAN_POINT('Ctrl Pts',(2.21480819795339E-15,-0.360330467682485,
-1.5183183843601));
#33108=CARTESIAN_POINT('Ctrl Pts',(2.22298984612665E-15,-0.346791235242338,
-1.51983853555761));
#33109=CARTESIAN_POINT('Ctrl Pts',(-7.06947890110157E-17,-0.333220577381782,
-1.52116970064367));
#33110=CARTESIAN_POINT('Ctrl Pts',(-1.38777878078145E-17,-0.319621170202027,
-1.52230829911641));
#33111=CARTESIAN_POINT('Ctrl Pts',(-0.62186969212423,-1.9522756157026,0.00152956335005719));
#33112=CARTESIAN_POINT('Ctrl Pts',(-0.596980647355082,-1.94905199344704,
-0.435857502745632));
#33113=CARTESIAN_POINT('Ctrl Pts',(-0.572091602585934,-1.80373720486496,
-0.875183433556484));
#33114=CARTESIAN_POINT('Ctrl Pts',(-0.547202557816786,-1.53382353634896,
-1.21572541890428));
#33115=CARTESIAN_POINT('Ctrl Pts',(-0.510189384479222,-1.13242760124485,
-1.72215463904135));
#33116=CARTESIAN_POINT('Ctrl Pts',(-0.473176211141658,-0.455475380096762,
-2.01011851545296));
#33117=CARTESIAN_POINT('Ctrl Pts',(-0.436163037804093,0.1877843306312,-1.94813338333444));
#33118=CARTESIAN_POINT('Ctrl Pts',(-0.399149864466528,0.831044041359161,
-1.88614825121591));
#33119=CARTESIAN_POINT('Ctrl Pts',(-0.36213669112896,1.44061124166701,-1.47421411056724));
#33120=CARTESIAN_POINT('Ctrl Pts',(-0.325123517791396,1.73785158268385,
-0.900376109039905));
#33121=CARTESIAN_POINT('Ctrl Pts',(-0.288110344453831,2.0350919237007,-0.326538107512548));
#33122=CARTESIAN_POINT('Ctrl Pts',(-0.25109717111627,2.02000540542655,0.409203754893459));
#33123=CARTESIAN_POINT('Ctrl Pts',(-0.214083997778705,1.69970343852974,
0.970348270842328));
#33124=CARTESIAN_POINT('Ctrl Pts',(-0.177070824441142,1.37940147163295,
1.53149278679117));
#33125=CARTESIAN_POINT('Ctrl Pts',(-0.140057651103576,0.753884056113526,
1.91803995628285));
#33126=CARTESIAN_POINT('Ctrl Pts',(-0.103044477766013,0.108541537644872,
1.95400482961695));
#33127=CARTESIAN_POINT('Ctrl Pts',(-0.0686963185106752,-0.490335175692911,
1.98738016832708));
#33128=CARTESIAN_POINT('Ctrl Pts',(-0.0343481592553384,-1.10628488527308,
1.7188407961645));
#33129=CARTESIAN_POINT('Ctrl Pts',(-1.90819582357449E-15,-1.495768828606,
1.26227079838508));
#33130=CARTESIAN_POINT('',(-19.646,-0.903606778650192,-1.26612599672285));
#33131=CARTESIAN_POINT('Ctrl Pts',(-19.646,-0.905542040608585,-1.26787934382136));
#33132=CARTESIAN_POINT('Ctrl Pts',(-19.646,-0.938681876239101,-1.25016622609516));
#33133=CARTESIAN_POINT('Ctrl Pts',(-19.646,-0.971073440107613,-1.23120562508964));
#33134=CARTESIAN_POINT('Ctrl Pts',(-19.646,-1.00263785675273,-1.21101354619544));
#33135=CARTESIAN_POINT('Ctrl Pts',(-19.646,-1.05261277003695,-1.17904408504205));
#33136=CARTESIAN_POINT('Ctrl Pts',(-19.646,-1.1005155382739,-1.14399043040363));
#33137=CARTESIAN_POINT('Ctrl Pts',(-19.646,-1.14626793887678,-1.10617282136889));
#33138=CARTESIAN_POINT('Ctrl Pts',(-19.646,-1.17314439188448,-1.08395752383931));
#33139=CARTESIAN_POINT('Ctrl Pts',(-19.646,-1.19927853253817,-1.06078746270321));
#33140=CARTESIAN_POINT('Ctrl Pts',(-19.646,-1.22465143234114,-1.03672005685037));
#33141=CARTESIAN_POINT('Ctrl Pts',(-19.646,-1.23635098556182,-1.02562247250465));
#33142=CARTESIAN_POINT('Ctrl Pts',(-19.646,-1.24789041542034,-1.01433201252715));
#33143=CARTESIAN_POINT('Ctrl Pts',(-19.646,-1.25925110031853,-1.00287136143659));
#33144=CARTESIAN_POINT('Ctrl Pts',(-19.646,-1.30312281878128,-0.958613602106813));
#33145=CARTESIAN_POINT('Ctrl Pts',(-19.646,-1.3443847292608,-0.911772278773441));
#33146=CARTESIAN_POINT('Ctrl Pts',(-19.646,-1.38294904546205,-0.862696554410881));
#33147=CARTESIAN_POINT('Ctrl Pts',(-19.646,-1.41264445582053,-0.824907118031911));
#33148=CARTESIAN_POINT('Ctrl Pts',(-19.646,-1.44074010106896,-0.785791596811784));
#33149=CARTESIAN_POINT('Ctrl Pts',(-19.646,-1.4671857543939,-0.745491044869591));
#33150=CARTESIAN_POINT('Ctrl Pts',(-19.646,-1.47620661389258,-0.731744149970738));
#33151=CARTESIAN_POINT('Ctrl Pts',(-19.646,-1.48503539940812,-0.717859249822184));
#33152=CARTESIAN_POINT('Ctrl Pts',(-19.646,-1.49366982591613,-0.703841592408462));
#33153=CARTESIAN_POINT('Ctrl Pts',(-19.646,-1.50209114300791,-0.69016990988787));
#33154=CARTESIAN_POINT('Ctrl Pts',(-19.646,-1.51032951371256,-0.676368303403145));
#33155=CARTESIAN_POINT('Ctrl Pts',(-19.646,-1.51836903542545,-0.662465935470385));
#33156=CARTESIAN_POINT('Ctrl Pts',(-19.646,-1.55076424157064,-0.606446424463152));
#33157=CARTESIAN_POINT('Ctrl Pts',(-19.646,-1.57997764506433,-0.548725277846029));
#33158=CARTESIAN_POINT('Ctrl Pts',(-19.646,-1.6059180737153,-0.489656925507297));
#33159=CARTESIAN_POINT('Ctrl Pts',(-19.646,-1.63239976292013,-0.429356081233618));
#33160=CARTESIAN_POINT('Ctrl Pts',(-19.646,-1.65547122307238,-0.367650443296635));
#33161=CARTESIAN_POINT('Ctrl Pts',(-19.646,-1.67500154178622,-0.304875460933321));
#33162=CARTESIAN_POINT('Ctrl Pts',(-19.646,-1.68790625616863,-0.263396710400418));
#33163=CARTESIAN_POINT('Ctrl Pts',(-19.646,-1.69926421211363,-0.221450247756649));
#33164=CARTESIAN_POINT('Ctrl Pts',(-19.646,-1.70902729549459,-0.17912585728895));
#33165=CARTESIAN_POINT('Ctrl Pts',(-19.646,-1.71381101181734,-0.158387749292715));
#33166=CARTESIAN_POINT('Ctrl Pts',(-19.646,-1.7182116941742,-0.137558839576148));
#33167=CARTESIAN_POINT('Ctrl Pts',(-19.646,-1.72222284706313,-0.116649366767487));
#33168=CARTESIAN_POINT('Ctrl Pts',(-19.646,-1.72468902535469,-0.103793589549136));
#33169=CARTESIAN_POINT('Ctrl Pts',(-19.646,-1.72700794401817,-0.0909073545491223));
#33170=CARTESIAN_POINT('Ctrl Pts',(-19.646,-1.72917798177892,-0.0779930136645168));
#33171=CARTESIAN_POINT('Ctrl Pts',(-19.646,-1.73099216263167,-0.0671964504052968));
#33172=CARTESIAN_POINT('Ctrl Pts',(-19.646,-1.73270181297803,-0.0563826288020671));
#33173=CARTESIAN_POINT('Ctrl Pts',(-19.646,-1.73430467550777,-0.0455638649458739));
#33174=CARTESIAN_POINT('Ctrl Pts',(-19.646,-1.74423506188351,0.0214627846927948));
#33175=CARTESIAN_POINT('Ctrl Pts',(-19.646,-1.75008999734432,0.0887933599084955));
#33176=CARTESIAN_POINT('Ctrl Pts',(-19.646,-1.75174634352653,0.156072973815415));
#33177=CARTESIAN_POINT('Ctrl Pts',(-19.646,-1.75216732819483,0.173173074173518));
#33178=CARTESIAN_POINT('Ctrl Pts',(-19.646,-1.75231686986298,0.190270032654354));
#33179=CARTESIAN_POINT('Ctrl Pts',(-19.646,-1.75219248471346,0.207358295798386));
#33180=CARTESIAN_POINT('Ctrl Pts',(-19.646,-1.75172041634255,0.272211926443289));
#33181=CARTESIAN_POINT('Ctrl Pts',(-19.646,-1.74730691088489,0.336939554811864));
#33182=CARTESIAN_POINT('Ctrl Pts',(-19.646,-1.73916871539667,0.401305845369932));
#33183=CARTESIAN_POINT('Ctrl Pts',(-19.646,-1.73475683721818,0.436200095963245));
#33184=CARTESIAN_POINT('Ctrl Pts',(-19.646,-1.72924938721083,0.470988342069356));
#33185=CARTESIAN_POINT('Ctrl Pts',(-19.646,-1.7226747045139,0.505633709783685));
#33186=CARTESIAN_POINT('Ctrl Pts',(-19.646,-1.7177037781737,0.531828064534477));
#33187=CARTESIAN_POINT('Ctrl Pts',(-19.646,-1.71212268625163,0.557940753879483));
#33188=CARTESIAN_POINT('Ctrl Pts',(-19.646,-1.70594210832947,0.58395576292157));
#33189=CARTESIAN_POINT('Ctrl Pts',(-19.646,-1.70239611990861,0.598881376997373));
#33190=CARTESIAN_POINT('Ctrl Pts',(-19.646,-1.69865150339267,0.613779102795182));
#33191=CARTESIAN_POINT('Ctrl Pts',(-19.646,-1.69471797730657,0.628617701099107));
#33192=CARTESIAN_POINT('Ctrl Pts',(-19.646,-1.67733891462321,0.694177436667802));
#33193=CARTESIAN_POINT('Ctrl Pts',(-19.646,-1.65625524843458,0.758681559480687));
#33194=CARTESIAN_POINT('Ctrl Pts',(-19.646,-1.63172440972949,0.821874451021119));
#33195=CARTESIAN_POINT('Ctrl Pts',(-19.646,-1.60667765966343,0.886396360744345));
#33196=CARTESIAN_POINT('Ctrl Pts',(-19.646,-1.57803704609287,0.949552185162904));
#33197=CARTESIAN_POINT('Ctrl Pts',(-19.646,-1.54602141156002,1.01107293048721));
#33198=CARTESIAN_POINT('Ctrl Pts',(-19.646,-1.51376408399581,1.07305810938115));
#33199=CARTESIAN_POINT('Ctrl Pts',(-19.646,-1.47808026191821,1.13338441161316));
#33200=CARTESIAN_POINT('Ctrl Pts',(-19.646,-1.43914228877744,1.19176565197817));
#33201=CARTESIAN_POINT('Ctrl Pts',(-19.646,-1.42928345262248,1.206547394243));
#33202=CARTESIAN_POINT('Ctrl Pts',(-19.646,-1.41921576123314,1.22120434749156));
#33203=CARTESIAN_POINT('Ctrl Pts',(-19.646,-1.40894153299102,1.23573163636577));
#33204=CARTESIAN_POINT('Ctrl Pts',(-19.646,-1.4015641455592,1.2461629248123));
#33205=CARTESIAN_POINT('Ctrl Pts',(-19.646,-1.39407933992703,1.25652845558403));
#33206=CARTESIAN_POINT('Ctrl Pts',(-19.646,-1.38649911575537,1.26681166279554));
#33207=CARTESIAN_POINT('Ctrl Pts',(-19.646,-1.34366530428306,1.32491930566387));
#33208=CARTESIAN_POINT('Ctrl Pts',(-19.646,-1.2977140106402,1.38050707160548));
#33209=CARTESIAN_POINT('Ctrl Pts',(-19.646,-1.2488866714459,1.4332945374332));
#33210=CARTESIAN_POINT('Ctrl Pts',(-19.646,-1.19994324988706,1.48620750045065));
#33211=CARTESIAN_POINT('Ctrl Pts',(-19.646,-1.14810965971326,1.53630784170276));
#33212=CARTESIAN_POINT('Ctrl Pts',(-19.646,-1.09357943713849,1.58329695308289));
#33213=CARTESIAN_POINT('Ctrl Pts',(-19.646,-1.04021055626029,1.62928532740834));
#33214=CARTESIAN_POINT('Ctrl Pts',(-19.646,-0.984258111839382,1.67229443841277));
#33215=CARTESIAN_POINT('Ctrl Pts',(-19.646,-0.925863744774077,1.71201523240195));
#33216=CARTESIAN_POINT('Ctrl Pts',(-19.646,-0.90473592603761,1.72638671680443));
#33217=CARTESIAN_POINT('Ctrl Pts',(-19.646,-0.883288096751299,1.74032739005835));
#33218=CARTESIAN_POINT('Ctrl Pts',(-19.646,-0.861525859670609,1.7538213116275));
#33219=CARTESIAN_POINT('Ctrl Pts',(-19.646,-0.90554204060855,-1.26787934382138));
#33220=CARTESIAN_POINT('Ctrl Pts',(-19.6116518407447,-0.515303398567461,
-1.54346439101212));
#33221=CARTESIAN_POINT('Ctrl Pts',(-19.5402905081518,0.58155483362262,-1.722138088561));
#33222=CARTESIAN_POINT('Ctrl Pts',(-19.4319160022213,1.77174315090552,-0.488859491694061));
#33223=CARTESIAN_POINT('Ctrl Pts',(-19.3208764822086,1.37253690144282,1.22265204623408));
#33224=CARTESIAN_POINT('Ctrl Pts',(-19.2098369621959,-0.281145520007231,
1.81625519837393));
#33225=CARTESIAN_POINT('Ctrl Pts',(-19.1201927262585,-1.40868791973966,
0.955800011746829));
#33226=CARTESIAN_POINT('Ctrl Pts',(-19.0675616636586,-1.554016444368,0.219461333177004));
#33227=CARTESIAN_POINT('Ctrl Pts',(-19.0519437743963,-1.55320700821059,
0.000650635102509029));
#33228=CARTESIAN_POINT('Origin',(-19.646,-2.59090492670967E-16,0.));
#33229=CARTESIAN_POINT('',(-19.646,-1.954,-2.39295984553393E-16));
#33230=CARTESIAN_POINT('Origin',(-19.646,0.,0.));
#33231=CARTESIAN_POINT('Origin',(-19.646,0.,0.));
#33232=CARTESIAN_POINT('',(-19.646,0.903606778650242,-1.26612599672281));
#33233=CARTESIAN_POINT('Ctrl Pts',(-19.646,0.863566768236388,1.75638951800437));
#33234=CARTESIAN_POINT('Ctrl Pts',(-19.646,0.903322736553012,1.7319792089365));
#33235=CARTESIAN_POINT('Ctrl Pts',(-19.646,0.942081600816466,1.706082519315));
#33236=CARTESIAN_POINT('Ctrl Pts',(-19.646,0.979747741712395,1.67869459433238));
#33237=CARTESIAN_POINT('Ctrl Pts',(-19.646,1.0378592801315,1.63644034643253));
#33238=CARTESIAN_POINT('Ctrl Pts',(-19.646,1.09337204689005,1.59063767529025));
#33239=CARTESIAN_POINT('Ctrl Pts',(-19.646,1.14612449678451,1.5416273763348));
#33240=CARTESIAN_POINT('Ctrl Pts',(-19.646,1.17160987932026,1.51794987472928));
#33241=CARTESIAN_POINT('Ctrl Pts',(-19.646,1.19645037254775,1.49352326161613));
#33242=CARTESIAN_POINT('Ctrl Pts',(-19.646,1.22062397437646,1.46838397290312));
#33243=CARTESIAN_POINT('Ctrl Pts',(-19.646,1.23081678670849,1.45778397817217));
#33244=CARTESIAN_POINT('Ctrl Pts',(-19.646,1.24089100137359,1.44705726575374));
#33245=CARTESIAN_POINT('Ctrl Pts',(-19.646,1.25084482785001,1.43620652381068));
#33246=CARTESIAN_POINT('Ctrl Pts',(-19.646,1.26039541734236,1.42579535357066));
#33247=CARTESIAN_POINT('Ctrl Pts',(-19.646,1.2698316591578,1.41527374749551));
#33248=CARTESIAN_POINT('Ctrl Pts',(-19.646,1.27914724914785,1.40465014664234));
#33249=CARTESIAN_POINT('Ctrl Pts',(-19.646,1.32621262813245,1.35097627296714));
#33250=CARTESIAN_POINT('Ctrl Pts',(-19.646,1.37024304194926,1.29465625509195));
#33251=CARTESIAN_POINT('Ctrl Pts',(-19.646,1.41107688405619,1.23602526535197));
#33252=CARTESIAN_POINT('Ctrl Pts',(-19.646,1.44042814800574,1.19388145603382));
#33253=CARTESIAN_POINT('Ctrl Pts',(-19.646,1.46812692994879,1.15054294882141));
#33254=CARTESIAN_POINT('Ctrl Pts',(-19.646,1.49409735999621,1.10612915663656));
#33255=CARTESIAN_POINT('Ctrl Pts',(-19.646,1.50834342473973,1.08176599600291));
#33256=CARTESIAN_POINT('Ctrl Pts',(-19.646,1.52206917616524,1.05707922579962));
#33257=CARTESIAN_POINT('Ctrl Pts',(-19.646,1.53526026066111,1.03208840623726));
#33258=CARTESIAN_POINT('Ctrl Pts',(-19.646,1.54099272219805,1.0212281231451));
#33259=CARTESIAN_POINT('Ctrl Pts',(-19.646,1.54662359108262,1.01031139276512));
#33260=CARTESIAN_POINT('Ctrl Pts',(-19.646,1.55214625633791,0.999351117833026));
#33261=CARTESIAN_POINT('Ctrl Pts',(-19.646,1.58348920551541,0.937147937975382));
#33262=CARTESIAN_POINT('Ctrl Pts',(-19.646,1.61140228754486,0.873447373552883));
#33263=CARTESIAN_POINT('Ctrl Pts',(-19.646,1.63573409282643,0.808558728131928));
#33264=CARTESIAN_POINT('Ctrl Pts',(-19.646,1.65948765101661,0.745212166006688));
#33265=CARTESIAN_POINT('Ctrl Pts',(-19.646,1.67982822719404,0.680732341235376));
#33266=CARTESIAN_POINT('Ctrl Pts',(-19.646,1.69656663148463,0.615401331854704));
#33267=CARTESIAN_POINT('Ctrl Pts',(-19.646,1.70778068689243,0.571632191958015));
#33268=CARTESIAN_POINT('Ctrl Pts',(-19.646,1.71737693174782,0.527480906477519));
#33269=CARTESIAN_POINT('Ctrl Pts',(-19.646,1.72528552443309,0.483033998311475));
#33270=CARTESIAN_POINT('Ctrl Pts',(-19.646,1.7316045497537,0.447520582802376));
#33271=CARTESIAN_POINT('Ctrl Pts',(-19.646,1.73684596146418,0.411818446376242));
#33272=CARTESIAN_POINT('Ctrl Pts',(-19.646,1.74096908581929,0.375973249752788));
#33273=CARTESIAN_POINT('Ctrl Pts',(-19.646,1.74271973989503,0.360753592483218));
#33274=CARTESIAN_POINT('Ctrl Pts',(-19.646,1.74426900447266,0.345503519836166));
#33275=CARTESIAN_POINT('Ctrl Pts',(-19.646,1.74561136180707,0.330255732772084));
#33276=CARTESIAN_POINT('Ctrl Pts',(-19.646,1.75132555048616,0.265348475971802));
#33277=CARTESIAN_POINT('Ctrl Pts',(-19.646,1.75330734745255,0.200390062729164));
#33278=CARTESIAN_POINT('Ctrl Pts',(-19.646,1.75138973772329,0.135641060055424));
#33279=CARTESIAN_POINT('Ctrl Pts',(-19.646,1.75083523799717,0.116918113617963));
#33280=CARTESIAN_POINT('Ctrl Pts',(-19.646,1.74995436364999,0.0982127193910304));
#33281=CARTESIAN_POINT('Ctrl Pts',(-19.646,1.74874226605705,0.079531327482009));
#33282=CARTESIAN_POINT('Ctrl Pts',(-19.646,1.74429950877487,0.0110575590098168));
#33283=CARTESIAN_POINT('Ctrl Pts',(-19.646,1.73541095028425,-0.0570958748323909));
#33284=CARTESIAN_POINT('Ctrl Pts',(-19.646,1.72226904404541,-0.124592446033735));
#33285=CARTESIAN_POINT('Ctrl Pts',(-19.646,1.71037294405752,-0.185690580905332));
#33286=CARTESIAN_POINT('Ctrl Pts',(-19.646,1.69499049540238,-0.246250814205604));
#33287=CARTESIAN_POINT('Ctrl Pts',(-19.646,1.6762313128498,-0.305997837855447));
#33288=CARTESIAN_POINT('Ctrl Pts',(-19.646,1.67266766774541,-0.317347862715789));
#33289=CARTESIAN_POINT('Ctrl Pts',(-19.646,1.66898472870697,-0.328659924368977));
#33290=CARTESIAN_POINT('Ctrl Pts',(-19.646,1.66518531160415,-0.339927647595734));
#33291=CARTESIAN_POINT('Ctrl Pts',(-19.646,1.64447516439434,-0.401346596984588));
#33292=CARTESIAN_POINT('Ctrl Pts',(-19.646,1.62029376539845,-0.46149556132515));
#33293=CARTESIAN_POINT('Ctrl Pts',(-19.646,1.59282690139432,-0.520099973095403));
#33294=CARTESIAN_POINT('Ctrl Pts',(-19.646,1.56548034847439,-0.578447684271151));
#33295=CARTESIAN_POINT('Ctrl Pts',(-19.646,1.53487629167091,-0.635265175881805));
#33296=CARTESIAN_POINT('Ctrl Pts',(-19.646,1.50115876935599,-0.690248721836702));
#33297=CARTESIAN_POINT('Ctrl Pts',(-19.646,1.46814035521906,-0.744092224158713));
#33298=CARTESIAN_POINT('Ctrl Pts',(-19.646,1.43213550204336,-0.796177659254549));
#33299=CARTESIAN_POINT('Ctrl Pts',(-19.646,1.39325288886873,-0.846177847660815));
#33300=CARTESIAN_POINT('Ctrl Pts',(-19.646,1.38629874007184,-0.855120372909513));
#33301=CARTESIAN_POINT('Ctrl Pts',(-19.646,1.37925248612795,-0.863996072867638));
#33302=CARTESIAN_POINT('Ctrl Pts',(-19.646,1.37211468424398,-0.872802907558143));
#33303=CARTESIAN_POINT('Ctrl Pts',(-19.646,1.3654767793905,-0.880992954254046));
#33304=CARTESIAN_POINT('Ctrl Pts',(-19.646,1.35876562654603,-0.88911612283082));
#33305=CARTESIAN_POINT('Ctrl Pts',(-19.646,1.35198260679088,-0.897170459130779));
#33306=CARTESIAN_POINT('Ctrl Pts',(-19.646,1.31202659151418,-0.944615283981971));
#33307=CARTESIAN_POINT('Ctrl Pts',(-19.646,1.26957231590532,-0.989683649287115));
#33308=CARTESIAN_POINT('Ctrl Pts',(-19.646,1.2247580044259,-1.03210786368823));
#33309=CARTESIAN_POINT('Ctrl Pts',(-19.646,1.18075456163743,-1.07376445573702));
#33310=CARTESIAN_POINT('Ctrl Pts',(-19.646,1.13447500920147,-1.1128722506342));
#33311=CARTESIAN_POINT('Ctrl Pts',(-19.646,1.08602704351211,-1.14913379788722));
#33312=CARTESIAN_POINT('Ctrl Pts',(-19.646,1.03912084562306,-1.18424138779347));
#33313=CARTESIAN_POINT('Ctrl Pts',(-19.646,0.990181444901801,-1.21668129711651));
#33314=CARTESIAN_POINT('Ctrl Pts',(-19.646,0.939294206718905,-1.24613612817705));
#33315=CARTESIAN_POINT('Ctrl Pts',(-19.646,0.927502678262808,-1.25296136552578));
#33316=CARTESIAN_POINT('Ctrl Pts',(-19.646,0.915606530740291,-1.25962610621517));
#33317=CARTESIAN_POINT('Ctrl Pts',(-19.646,0.903606778650211,-1.26612599672283));
#33318=CARTESIAN_POINT('Origin',(-19.646,0.,0.));
#33319=CARTESIAN_POINT('Origin',(-20.9400562256037,0.,0.));
#33320=CARTESIAN_POINT('Ctrl Pts',(-19.646,0.903606778650211,-1.26612599672283));
#33321=CARTESIAN_POINT('Ctrl Pts',(-19.6089868266624,1.32425114367218,-0.965921198291487));
#33322=CARTESIAN_POINT('Ctrl Pts',(-19.5349604799873,1.83563729847737,0.081414173630813));
#33323=CARTESIAN_POINT('Ctrl Pts',(-19.4239209599746,0.926784913186551,
1.58861167214729));
#33324=CARTESIAN_POINT('Ctrl Pts',(-19.3128814399619,-0.829751980945401,
1.63941117334604));
#33325=CARTESIAN_POINT('Ctrl Pts',(-19.234926528505,-1.53031391152993,0.624960285503497));
#33326=CARTESIAN_POINT('Ctrl Pts',(-19.1939847903856,-1.55770722541468,
0.0556933182705827));
#33327=CARTESIAN_POINT('Ctrl Pts',(-19.1900562256037,-1.55732260026824,
0.00102952447757978));
#33328=CARTESIAN_POINT('Ctrl Pts',(-19.8760740822721,1.13509973994379,-1.59049193030947));
#33329=CARTESIAN_POINT('Ctrl Pts',(-19.8390609089345,1.66350802618803,-1.21337834873771));
#33330=CARTESIAN_POINT('Ctrl Pts',(-19.7650345622594,2.30590503453859,0.102271485229633));
#33331=CARTESIAN_POINT('Ctrl Pts',(-19.6539950422467,1.16421582794371,1.9955944759729));
#33332=CARTESIAN_POINT('Ctrl Pts',(-19.542955522234,-1.04232424993082,2.05940818561114));
#33333=CARTESIAN_POINT('Ctrl Pts',(-19.4319160022213,-2.29585551567116,
0.244228327910747));
#33334=CARTESIAN_POINT('Ctrl Pts',(-19.3208764822086,-1.45163427674195,
-1.79566928904087));
#33335=CARTESIAN_POINT('Ctrl Pts',(-19.2098369621959,0.719270307589218,
-2.19382897651929));
#33336=CARTESIAN_POINT('Ctrl Pts',(-19.0987974421832,2.23281233943022,-0.587628905444012));
#33337=CARTESIAN_POINT('Ctrl Pts',(-18.9877579221705,1.70598616341913,1.55578514652744));
#33338=CARTESIAN_POINT('Ctrl Pts',(-18.8767184021578,-0.379838299429391,
2.27736225800791));
#33339=CARTESIAN_POINT('Ctrl Pts',(-18.7656788821451,-2.11854523576817,
0.917883122180374));
#33340=CARTESIAN_POINT('Ctrl Pts',(-18.6546393621324,-1.92127159556107,
-1.28041564965079));
#33341=CARTESIAN_POINT('Ctrl Pts',(-18.5435998421198,0.03171693881648,-2.30861767801051));
#33342=CARTESIAN_POINT('Ctrl Pts',(-18.432560322107,1.95572010220925,-1.22714892034321));
#33343=CARTESIAN_POINT('Ctrl Pts',(-18.3215208020944,2.09253210076758,0.975727678888284));
#33344=CARTESIAN_POINT('Ctrl Pts',(-18.2104812820816,0.317129050815823,
2.28695445182457));
#33345=CARTESIAN_POINT('Ctrl Pts',(-18.099441762069,-1.74807521169763,1.50829928845439));
#33346=CARTESIAN_POINT('Ctrl Pts',(-17.9884022420563,-2.21583935163955,
-0.648682819590979));
#33347=CARTESIAN_POINT('Ctrl Pts',(-17.8773627220436,-0.658707176843674,
-2.21287998534429));
#33348=CARTESIAN_POINT('Ctrl Pts',(-17.7663232020309,1.50037008987612,-1.75488543793783));
#33349=CARTESIAN_POINT('Ctrl Pts',(-17.6552836820182,2.28836703304007,0.306772824349375));
#33350=CARTESIAN_POINT('Ctrl Pts',(-17.5442441620055,0.985189881382429,
2.08809340919601));
#33351=CARTESIAN_POINT('Ctrl Pts',(-17.4332046419928,-1.21828145781376,
1.96125559954424));
#33352=CARTESIAN_POINT('Ctrl Pts',(-17.3221651219801,-2.30845297604624,
0.0421673077566786));
#33353=CARTESIAN_POINT('Ctrl Pts',(-17.2111256019674,-1.28909530809731,
-1.91545464701142));
#33354=CARTESIAN_POINT('Ctrl Pts',(-17.1000860819548,0.908273868493995,
-2.12268033511088));
#33355=CARTESIAN_POINT('Ctrl Pts',(-16.989046561942,2.27563686670409,-0.390141094771527));
#33356=CARTESIAN_POINT('Ctrl Pts',(-16.8780070419294,1.56345896252262,1.69892003778701));
#33357=CARTESIAN_POINT('Ctrl Pts',(-16.7669675219166,-0.577451666473502,
2.23546030968653));
#33358=CARTESIAN_POINT('Ctrl Pts',(-16.655928001904,-2.19067073934843,0.729174145634008));
#33359=CARTESIAN_POINT('Ctrl Pts',(-16.5448884818913,-1.80199334427159,
-1.44345183849261));
#33360=CARTESIAN_POINT('Ctrl Pts',(-16.4338489618786,0.233396195306619,
-2.29701097929521));
#33361=CARTESIAN_POINT('Ctrl Pts',(-16.3228094418659,2.05550173441762,-1.05149695326574));
#33362=CARTESIAN_POINT('Ctrl Pts',(-16.2117699218532,1.99923203984308,1.15490453016024));
#33363=CARTESIAN_POINT('Ctrl Pts',(-16.1007304018405,0.116007939373285,
2.30592180720441));
#33364=CARTESIAN_POINT('Ctrl Pts',(-15.9896908818278,-1.8732274753089,1.34972295256322));
#33365=CARTESIAN_POINT('Ctrl Pts',(-15.8786513618151,-2.150654995229,-0.839890656231781));
#33366=CARTESIAN_POINT('Ctrl Pts',(-15.7676118418024,-0.462753558433016,
-2.26198858686089));
#33367=CARTESIAN_POINT('Ctrl Pts',(-15.6565723217897,1.6480250809965,-1.61701779685203));
#33368=CARTESIAN_POINT('Ctrl Pts',(-15.545532801777,2.25279210058805,0.505629285601668));
#33369=CARTESIAN_POINT('Ctrl Pts',(-15.4344932817643,0.798894407071541,
2.16621812135345));
#33370=CARTESIAN_POINT('Ctrl Pts',(-15.3234537617516,-1.38505544035138,
1.84725597849434));
#33371=CARTESIAN_POINT('Ctrl Pts',(-15.212414241739,-2.30330271361953,-0.159780575674832));
#33372=CARTESIAN_POINT('Ctrl Pts',(-15.1013747217263,-1.11672725650928,
-2.02080515079989));
#33373=CARTESIAN_POINT('Ctrl Pts',(-14.9903352017136,1.09034494175236,-2.03516120514448));
#33374=CARTESIAN_POINT('Ctrl Pts',(-14.8792956817009,2.30102929929156,-0.189729772919033));
#33375=CARTESIAN_POINT('Ctrl Pts',(-14.7682561616882,1.40896843633621,1.82908205620699));
#33376=CARTESIAN_POINT('Ctrl Pts',(-14.6572166416755,-0.770647368334038,
2.17642731480055));
#33377=CARTESIAN_POINT('Ctrl Pts',(-14.5461771216628,-2.24602395668922,
0.534892146986835));
#33378=CARTESIAN_POINT('Ctrl Pts',(-14.4351376016501,-1.66892075198025,
-1.59544249239507));
#33379=CARTESIAN_POINT('Ctrl Pts',(-14.3240980816374,0.433289123769849,
-2.26781695869681));
#33380=CARTESIAN_POINT('Ctrl Pts',(-14.2130585616247,2.13954722507716,-0.867796574431303));
#33381=CARTESIAN_POINT('Ctrl Pts',(-14.102019041612,1.89062696210268,1.32524070006188));
#33382=CARTESIAN_POINT('Ctrl Pts',(-13.9909795215993,-0.0860013354994131,
2.30723579055597));
#33383=CARTESIAN_POINT('Ctrl Pts',(-13.8799400015866,-1.98403919653764,
1.18081399446837));
#33384=CARTESIAN_POINT('Ctrl Pts',(-13.768900481574,-2.0690062987299,-1.02466880441734));
#33385=CARTESIAN_POINT('Ctrl Pts',(-13.6578609615612,-0.263257316964935,
-2.29378046203086));
#33386=CARTESIAN_POINT('Ctrl Pts',(-13.5468214415486,1.78306359718642,-1.46677109029281));
#33387=CARTESIAN_POINT('Ctrl Pts',(-13.4357819215358,2.19997090153458,0.700614912295794));
#33388=CARTESIAN_POINT('Ctrl Pts',(-13.3247424015232,0.606482988467133,
2.22775932444016));
#33389=CARTESIAN_POINT('Ctrl Pts',(-13.2137028815105,-1.5412261184387,1.71911467760951));
#33390=CARTESIAN_POINT('Ctrl Pts',(-13.1026633614978,-2.28051949798023,
-0.360505259687157));
#33391=CARTESIAN_POINT('Ctrl Pts',(-12.9916238414851,-0.935810089682886,
-2.11068536238299));
#33392=CARTESIAN_POINT('Ctrl Pts',(-12.8805843214724,1.26406886990054,-1.93206188179325));
#33393=CARTESIAN_POINT('Ctrl Pts',(-12.7695448014597,2.30880618249247,0.0121340271403076));
#33394=CARTESIAN_POINT('Ctrl Pts',(-12.658505281447,1.24369154023141,1.94524152117081));
#33395=CARTESIAN_POINT('Ctrl Pts',(-12.5474657614343,-0.95794337267385,
2.10073266211585));
#33396=CARTESIAN_POINT('Ctrl Pts',(-12.4364262414216,-2.28418271846725,
0.336515276897891));
#33397=CARTESIAN_POINT('Ctrl Pts',(-12.3253867214089,-1.52307172262353,
-1.73521922265594));
#33398=CARTESIAN_POINT('Ctrl Pts',(-12.2143472013963,0.629865003645723,
-2.22126164602743));
#33399=CARTESIAN_POINT('Ctrl Pts',(-12.1033076813835,2.20721339369492,-0.677452771507981));
#33400=CARTESIAN_POINT('Ctrl Pts',(-11.9922681613709,1.76754817351653,1.48543147846963));
#33401=CARTESIAN_POINT('Ctrl Pts',(-11.8812286413582,-0.287352226413828,
2.29088671062214));
#33402=CARTESIAN_POINT('Ctrl Pts',(-11.7701891213455,-2.07966208876338,
1.00286530475953));
#33403=CARTESIAN_POINT('Ctrl Pts',(-11.6591496013328,-1.97151830685153,
-1.2016025918245));
#33404=CARTESIAN_POINT('Ctrl Pts',(-11.5481100813201,-0.0617457068599174,
-2.30801228129628));
#33405=CARTESIAN_POINT('Ctrl Pts',(-11.4370705613074,1.90445185478939,-1.30529550513259));
#33406=CARTESIAN_POINT('Ctrl Pts',(-11.3260310412947,2.13030780646733,0.890236975548903));
#33407=CARTESIAN_POINT('Ctrl Pts',(-11.214991521282,0.409428634168118,2.2722458970044));
#33408=CARTESIAN_POINT('Ctrl Pts',(-11.1039520012693,-1.68559792682173,
1.57781267963734));
#33409=CARTESIAN_POINT('Ctrl Pts',(-10.9929124812566,-2.24027774585957,
-0.558470092606996));
#33410=CARTESIAN_POINT('Ctrl Pts',(-10.8818729612439,-0.74772882072763,
-2.18440720415937));
#33411=CARTESIAN_POINT('Ctrl Pts',(-10.7708334412313,1.42811570802619,-1.81417164221552));
#33412=CARTESIAN_POINT('Ctrl Pts',(-10.6597939212185,2.29890798025732,0.213904935051304));
#33413=CARTESIAN_POINT('Ctrl Pts',(-10.5487544012059,1.06889355292529,2.04650917306638));
#33414=CARTESIAN_POINT('Ctrl Pts',(-10.4377148811932,-1.13790583334797,
2.00895583260627));
#33415=CARTESIAN_POINT('Ctrl Pts',(-10.3266753611805,-2.30485489994822,
0.135562211234455));
#33416=CARTESIAN_POINT('Ctrl Pts',(-10.2156358411678,-1.36556280469463,
-1.86171196734742));
#33417=CARTESIAN_POINT('Ctrl Pts',(-10.1045963211551,0.821618946610189,
-2.15770144586809));
#33418=CARTESIAN_POINT('Ctrl Pts',(-9.99355680114238,2.25798222133836,-0.481922723110236));
#33419=CARTESIAN_POINT('Ctrl Pts',(-9.88251728112969,1.63093790480174,1.6342505235156));
#33420=CARTESIAN_POINT('Ctrl Pts',(-9.77147776111699,-0.48650328990636,
2.25699972792208));
#33421=CARTESIAN_POINT('Ctrl Pts',(-9.6604382411043,-2.15936411011838,0.817239171150482));
#33422=CARTESIAN_POINT('Ctrl Pts',(-9.5493987210916,-1.85893733974787,-1.36933750033409));
#33423=CARTESIAN_POINT('Ctrl Pts',(-9.43835920107892,0.140238598030964,
-2.30457509284302));
#33424=CARTESIAN_POINT('Ctrl Pts',(-9.32731968106622,2.01126056496325,-1.13382721909196));
#33425=CARTESIAN_POINT('Ctrl Pts',(-9.21628016105352,2.04433612180518,1.0730438220374));
#33426=CARTESIAN_POINT('Ctrl Pts',(-9.10524064104083,0.209239895465708,
2.29933727171017));
#33427=CARTESIAN_POINT('Ctrl Pts',(-8.99420112102815,-1.81706562588916,
1.42443172322934));
#33428=CARTESIAN_POINT('Ctrl Pts',(-8.88316160101544,-2.18288552833439,
-0.752159552966248));
#33429=CARTESIAN_POINT('Ctrl Pts',(-8.77212208100277,-0.553923307403332,
-2.24140629794008));
#33430=CARTESIAN_POINT('Ctrl Pts',(-8.66108256099004,1.58122959415986,-1.6823929961466));
#33431=CARTESIAN_POINT('Ctrl Pts',(-8.55004304097738,2.2714104683578,0.414038291906306));
#33432=CARTESIAN_POINT('Ctrl Pts',(-8.43900352096466,0.88591264190158,2.1321097565203));
#33433=CARTESIAN_POINT('Ctrl Pts',(-8.32796400095198,-1.30915704620272,
1.90179942457344));
#33434=CARTESIAN_POINT('Ctrl Pts',(-8.21692448093929,-2.30788224507037,
-0.0664286520941292));
#33435=CARTESIAN_POINT('Ctrl Pts',(-8.1058849609266,-1.19759980905913,-1.9739523601829));
#33436=CARTESIAN_POINT('Ctrl Pts',(-7.9948454409139,1.00708297871625,-2.07762294387363));
#33437=CARTESIAN_POINT('Ctrl Pts',(-7.88380592090121,2.29146504681414,-0.282703311192433));
#33438=CARTESIAN_POINT('Ctrl Pts',(-7.77276640088852,1.48184197703646,1.77055854973022));
#33439=CARTESIAN_POINT('Ctrl Pts',(-7.66172688087582,-0.68192992331063,
2.20583426454112));
#33440=CARTESIAN_POINT('Ctrl Pts',(-7.55068736086314,-2.2225351010979,0.62535665609143));
#33441=CARTESIAN_POINT('Ctrl Pts',(-7.43964784085043,-1.73212526197346,
-1.52658943392238));
#33442=CARTESIAN_POINT('Ctrl Pts',(-7.32860832083775,0.341149305137663,
-2.28349521009661));
#33443=CARTESIAN_POINT('Ctrl Pts',(-7.21756880082505,2.10267205271563,-0.953678909098191));
#33444=CARTESIAN_POINT('Ctrl Pts',(-7.10652928081236,1.94271400451386,1.24763597238771));
#33445=CARTESIAN_POINT('Ctrl Pts',(-6.99548976079966,0.00744931895763328,
2.3088260503072));
#33446=CARTESIAN_POINT('Ctrl Pts',(-6.88445024078697,-1.9346227635487,1.26014601760641));
#33447=CARTESIAN_POINT('Ctrl Pts',(-6.77341072077428,-2.10878221201579,
-0.940090849448));
#33448=CARTESIAN_POINT('Ctrl Pts',(-6.66237120076159,-0.355877229471387,
-2.28124628667617));
#33449=CARTESIAN_POINT('Ctrl Pts',(-6.55133168074889,1.72223836363943,-1.53773477613621));
#33450=CARTESIAN_POINT('Ctrl Pts',(-6.4402921607362,2.22652415423095,0.611001975083735));
#33451=CARTESIAN_POINT('Ctrl Pts',(-6.32925264072351,0.69614961908643,2.2013879555353));
#33452=CARTESIAN_POINT('Ctrl Pts',(-6.21821312071081,-1.47038599611639,
1.78008377481369));
#33453=CARTESIAN_POINT('Ctrl Pts',(-6.10717360069812,-2.29324157796728,
-0.267910970309621));
#33454=CARTESIAN_POINT('Ctrl Pts',(-5.99613408068543,-1.02046857786368,
-2.07108114387703));
#33455=CARTESIAN_POINT('Ctrl Pts',(-5.88509456067273,1.18483727848316,-1.98163918169952));
#33456=CARTESIAN_POINT('Ctrl Pts',(-5.77405504066004,2.30740554206606,-0.0813196616628663));
#33457=CARTESIAN_POINT('Ctrl Pts',(-5.66301552064734,1.32140179536823,1.89331204985541));
#33458=CARTESIAN_POINT('Ctrl Pts',(-5.55197600063466,-0.872136036366616,
2.13778201812083));
#33459=CARTESIAN_POINT('Ctrl Pts',(-5.44093648062196,-2.26869145564129,
0.428686717814187));
#33460=CARTESIAN_POINT('Ctrl Pts',(-5.32989696060927,-1.59205288447209,
-1.67215454906962));
#33461=CARTESIAN_POINT('Ctrl Pts',(-5.21885744059657,0.539448340827144,
-2.24493401027935));
#33462=CARTESIAN_POINT('Ctrl Pts',(-5.10781792058389,2.17798651662185,-0.766229702076018));
#33463=CARTESIAN_POINT('Ctrl Pts',(-4.99677840057118,1.82621942357963,1.41267683490264));
#33464=CARTESIAN_POINT('Ctrl Pts',(-4.8857388805585,-0.194398285875258,
2.30063959136994));
#33465=CARTESIAN_POINT('Ctrl Pts',(-4.7746993605458,-2.03736938012958,1.08621325339021));
#33466=CARTESIAN_POINT('Ctrl Pts',(-4.66365984053311,-2.01853509547436,
-1.12082527240798));
#33467=CARTESIAN_POINT('Ctrl Pts',(-4.55262032052042,-0.155106730371774,
-2.30362217499385));
#33468=CARTESIAN_POINT('Ctrl Pts',(-4.44158080050772,1.85006252262662,-1.38130441442235));
#33469=CARTESIAN_POINT('Ctrl Pts',(-4.33054128049504,2.16459266543765,0.803288127425982));
#33470=CARTESIAN_POINT('Ctrl Pts',(-4.21950176048233,0.501057216920676,
2.25381341026746));
#33471=CARTESIAN_POINT('Ctrl Pts',(-4.10846224046965,-1.62035839348706,
1.64474067852272));
#33472=CARTESIAN_POINT('Ctrl Pts',(-3.99742272045695,-2.26104498039055,
-0.467342293805651));
#33473=CARTESIAN_POINT('Ctrl Pts',(-3.88638320044426,-0.835525140761208,
-2.15235474819651));
#33474=CARTESIAN_POINT('Ctrl Pts',(-3.77534368043157,1.35352104635311,-1.8704849638577));
#33475=CARTESIAN_POINT('Ctrl Pts',(-3.66430416041887,2.30568167449427,0.120686531233159));
#33476=CARTESIAN_POINT('Ctrl Pts',(-3.55326464040618,1.15084561098174,2.00157128341837));
#33477=CARTESIAN_POINT('Ctrl Pts',(-3.44222512039349,-1.055665504561,2.05336396322383));
#33478=CARTESIAN_POINT('Ctrl Pts',(-3.3311856003808,-2.29747982336605,0.228734964692146));
#33479=CARTESIAN_POINT('Ctrl Pts',(-3.2201460803681,-1.43979253255639,-1.80491847076076));
#33480=CARTESIAN_POINT('Ctrl Pts',(-3.10910656035541,0.733617625198351,
-2.18918669904949));
#33481=CARTESIAN_POINT('Ctrl Pts',(-2.99806704034272,2.23662738604792,-0.572914616908127));
#33482=CARTESIAN_POINT('Ctrl Pts',(-2.88702752033002,1.69574420447561,1.56690293761921));
#33483=CARTESIAN_POINT('Ctrl Pts',(-2.77598800031733,-0.394757673379551,
2.27484056684494));
#33484=CARTESIAN_POINT('Ctrl Pts',(-2.66494848030463,-2.12451889725514,
0.903964973503894));
#33485=CARTESIAN_POINT('Ctrl Pts',(-2.55390896029194,-1.91283506775852,
-1.29297920633453));
#33486=CARTESIAN_POINT('Ctrl Pts',(-2.44286944027925,0.0468511924372969,
-2.30836266712224));
#33487=CARTESIAN_POINT('Ctrl Pts',(-2.33182992026656,1.96372350683224,-1.21429945920298));
#33488=CARTESIAN_POINT('Ctrl Pts',(-2.22079040025386,2.08609012919687,0.989424689671358));
#33489=CARTESIAN_POINT('Ctrl Pts',(-2.10975088024117,0.302128947588233,
2.28898479809507));
#33490=CARTESIAN_POINT('Ctrl Pts',(-1.99871136022848,-1.75792608649789,
1.49680621617262));
#33491=CARTESIAN_POINT('Ctrl Pts',(-1.88767184021578,-2.21153900378128,
-0.663195798735933));
#33492=CARTESIAN_POINT('Ctrl Pts',(-1.77663232020309,-0.644185200405014,
-2.21715112630666));
#33493=CARTESIAN_POINT('Ctrl Pts',(-1.6655928001904,1.51184266846055,-1.74501095853683));
#33494=CARTESIAN_POINT('Ctrl Pts',(-1.55455328017771,2.28630712417556,0.321768286248855));
#33495=CARTESIAN_POINT('Ctrl Pts',(-1.44351376016501,0.971478199189345,
2.09450846247627));
#33496=CARTESIAN_POINT('Ctrl Pts',(-1.33247424015232,-1.2311115678387,1.9532244763376));
#33497=CARTESIAN_POINT('Ctrl Pts',(-1.22143472013963,-2.3086831418981,0.0270357188913206));
#33498=CARTESIAN_POINT('Ctrl Pts',(-1.11039520012693,-1.27650350580558,
-1.92387165415099));
#33499=CARTESIAN_POINT('Ctrl Pts',(-0.999355680114239,0.922158647667554,
-2.11666705375319));
#33500=CARTESIAN_POINT('Ctrl Pts',(-0.888316160101547,2.27816865573076,
-0.375238308250741));
#33501=CARTESIAN_POINT('Ctrl Pts',(-0.777276640088857,1.55224358940625,
1.7091806553938));
#33502=CARTESIAN_POINT('Ctrl Pts',(-0.666237120076159,-0.592012005603808,
2.23153694542934));
#33503=CARTESIAN_POINT('Ctrl Pts',(-0.555197600063465,-2.1955620628257,
0.714966780555073));
#33504=CARTESIAN_POINT('Ctrl Pts',(-0.444158080050777,-1.79219063562177,
-1.45555925698041));
#33505=CARTESIAN_POINT('Ctrl Pts',(-0.33311856003808,0.247876640334474,
-2.29481134042266));
#33506=CARTESIAN_POINT('Ctrl Pts',(-0.22207904002539,2.0634575466964,-1.03920101979834));
#33507=CARTESIAN_POINT('Ctrl Pts',(-0.111039520012697,1.98938703685113,
1.170468582496));
#33508=CARTESIAN_POINT('Ctrl Pts',(-0.0370131733375646,0.733938965798303,
1.92376702457974));
#33509=CARTESIAN_POINT('Ctrl Pts',(0.,0.0853826423430472,1.95213365433479));
#33510=CARTESIAN_POINT('Ctrl Pts',(-19.7993827215147,1.0579354195126,-1.48236995244726));
#33511=CARTESIAN_POINT('Ctrl Pts',(-19.7623695481771,1.55042239868275,-1.1308926319223));
#33512=CARTESIAN_POINT('Ctrl Pts',(-19.688343201502,2.14914912251819,0.0953190480300262));
#33513=CARTESIAN_POINT('Ctrl Pts',(-19.5773036814893,1.08507218969133,1.85993354136436));
#33514=CARTESIAN_POINT('Ctrl Pts',(-19.4662641614766,-0.971466826935683,
1.91940918152277));
#33515=CARTESIAN_POINT('Ctrl Pts',(-19.3552246414639,-2.13978277206915,
0.227625634517308));
#33516=CARTESIAN_POINT('Ctrl Pts',(-19.2441851214512,-1.35295187154209,
-1.67359931093053));
#33517=CARTESIAN_POINT('Ctrl Pts',(-19.1331456014385,0.670374159930676,
-2.0446920186307));
#33518=CARTESIAN_POINT('Ctrl Pts',(-19.0221060814259,2.08102528428471,-0.547681768149684));
#33519=CARTESIAN_POINT('Ctrl Pts',(-18.9110665614132,1.59001286315942,1.4500225431683));
#33520=CARTESIAN_POINT('Ctrl Pts',(-18.8000270414005,-0.354016811486251,
2.12254668997377));
#33521=CARTESIAN_POINT('Ctrl Pts',(-18.6889875213878,-1.97452608250074,
0.855485233373004));
#33522=CARTESIAN_POINT('Ctrl Pts',(-18.5779480013751,-1.79066314608461,
-1.19337272293876));
#33523=CARTESIAN_POINT('Ctrl Pts',(-18.4669084813624,0.0295608146065764,
-2.15167735991307));
#33524=CARTESIAN_POINT('Ctrl Pts',(-18.3558689613497,1.82276983596386,-1.14372707715715));
#33525=CARTESIAN_POINT('Ctrl Pts',(-18.244829441337,1.95028132592011,0.909397504879913));
#33526=CARTESIAN_POINT('Ctrl Pts',(-18.1337899213243,0.295570550858466,
2.13148680442571));
#33527=CARTESIAN_POINT('Ctrl Pts',(-18.0227504013116,-1.62924068903274,
1.40576478377186));
#33528=CARTESIAN_POINT('Ctrl Pts',(-17.9117108812989,-2.06520612379439,
-0.604585224298059));
#33529=CARTESIAN_POINT('Ctrl Pts',(-17.8006713612862,-0.613928123624273,
-2.06244793584588));
#33530=CARTESIAN_POINT('Ctrl Pts',(-17.6896318412735,1.39837461379019,-1.63558795465258));
#33531=CARTESIAN_POINT('Ctrl Pts',(-17.5785923212608,2.13280335807138,0.285918342857852));
#33532=CARTESIAN_POINT('Ctrl Pts',(-17.4675528012481,0.918216464846976,
1.94614437754049));
#33533=CARTESIAN_POINT('Ctrl Pts',(-17.3565132812355,-1.13546242660618,
1.8279290290191));
#33534=CARTESIAN_POINT('Ctrl Pts',(-17.2454737612228,-2.15152385442317,
0.0393007652556636));
#33535=CARTESIAN_POINT('Ctrl Pts',(-17.1344342412101,-1.20146233636809,
-1.78524163492781));
#33536=CARTESIAN_POINT('Ctrl Pts',(-17.0233947211974,0.846529218784861,
-1.97838007691544));
#33537=CARTESIAN_POINT('Ctrl Pts',(-16.9123552011847,2.12093859113575,-0.363619220621685));
#33538=CARTESIAN_POINT('Ctrl Pts',(-16.801315681172,1.4571746915289,1.58342709424245));
#33539=CARTESIAN_POINT('Ctrl Pts',(-16.6902761611593,-0.53819638003717,
2.08349324496288));
#33540=CARTESIAN_POINT('Ctrl Pts',(-16.5792366411466,-2.04174847909078,
0.679604732970229));
#33541=CARTESIAN_POINT('Ctrl Pts',(-16.4681971211339,-1.67949345554894,
-1.34532567717577));
#33542=CARTESIAN_POINT('Ctrl Pts',(-16.3571576011212,0.217529872578918,
-2.14085968703163));
#33543=CARTESIAN_POINT('Ctrl Pts',(-16.2461180811086,1.91576829170772,-0.980015967957599));
#33544=CARTESIAN_POINT('Ctrl Pts',(-16.1350785610958,1.8633238228732,1.07639387590079));
#33545=CARTESIAN_POINT('Ctrl Pts',(-16.0240390410832,0.108121695115326,
2.14916475497463));
#33546=CARTESIAN_POINT('Ctrl Pts',(-15.9129995210704,-1.74588507529003,
1.25796850073853));
#33547=CARTESIAN_POINT('Ctrl Pts',(-15.8019600010578,-2.0044530137212,-0.782794711757463));
#33548=CARTESIAN_POINT('Ctrl Pts',(-15.6909204810451,-0.431295473643615,
-2.10821812424334));
#33549=CARTESIAN_POINT('Ctrl Pts',(-15.5798809610324,1.53599198738047,-1.50709258497119));
#33550=CARTESIAN_POINT('Ctrl Pts',(-15.4688414410197,2.09964681705268,0.471256499809728));
#33551=CARTESIAN_POINT('Ctrl Pts',(-15.357801921007,0.744585396287178,2.0189581552396));
#33552=CARTESIAN_POINT('Ctrl Pts',(-15.2467624009943,-1.29089907853287,
1.72167912632273));
#33553=CARTESIAN_POINT('Ctrl Pts',(-15.1357228809816,-2.14672370792567,
-0.148918658341753));
#33554=CARTESIAN_POINT('Ctrl Pts',(-15.0246833609689,-1.04081190138835,
-1.88343038918375));
#33555=CARTESIAN_POINT('Ctrl Pts',(-14.9136438409562,1.01622306196928,-1.89681051591725));
#33556=CARTESIAN_POINT('Ctrl Pts',(-14.8026043209435,2.14460484078461,-0.176831902822113));
#33557=CARTESIAN_POINT('Ctrl Pts',(-14.6915648009308,1.31318646399232,1.70474067111682));
#33558=CARTESIAN_POINT('Ctrl Pts',(-14.5805252809181,-0.718258597218173,
2.0284733255566));
#33559=CARTESIAN_POINT('Ctrl Pts',(-14.4694857609054,-2.09333877300777,
0.498530065687933));
#33560=CARTESIAN_POINT('Ctrl Pts',(-14.3584462408927,-1.55546716623066,
-1.48698397427506));
#33561=CARTESIAN_POINT('Ctrl Pts',(-14.24740672088,0.403834037481487,-2.11365028212897));
#33562=CARTESIAN_POINT('Ctrl Pts',(-14.1363672008674,1.99410035213392,-0.808803579734818));
#33563=CARTESIAN_POINT('Ctrl Pts',(-14.0253276808547,1.76210174129103,1.23515055694098));
#33564=CARTESIAN_POINT('Ctrl Pts',(-13.914288160842,-0.0801549465201214,
2.15038941346001));
#33565=CARTESIAN_POINT('Ctrl Pts',(-13.8032486408293,-1.84916379226943,
1.10054200934459));
#33566=CARTESIAN_POINT('Ctrl Pts',(-13.6922091208166,-1.92835481288141,
-0.955011602342901));
#33567=CARTESIAN_POINT('Ctrl Pts',(-13.5811696008039,-0.245361028870353,
-2.13784878101426));
#33568=CARTESIAN_POINT('Ctrl Pts',(-13.4701300807912,1.66185055667484,-1.36705968130584));
#33569=CARTESIAN_POINT('Ctrl Pts',(-13.3590905607785,2.05041641428424,0.652986962355509));
#33570=CARTESIAN_POINT('Ctrl Pts',(-13.2480510407658,0.565254146620652,
2.07631577432255));
#33571=CARTESIAN_POINT('Ctrl Pts',(-13.1370115207531,-1.43645324088873,
1.60224889817803));
#33572=CARTESIAN_POINT('Ctrl Pts',(-13.0259720007404,-2.12548930010491,
-0.335998035875247));
#33573=CARTESIAN_POINT('Ctrl Pts',(-12.9149324807277,-0.87219352183257,
-1.9672005249709));
#33574=CARTESIAN_POINT('Ctrl Pts',(-12.803892960715,1.1781372007338,-1.80071990637623));
#33575=CARTESIAN_POINT('Ctrl Pts',(-12.6928534407024,2.15185304982047,0.0113091534085617));
#33576=CARTESIAN_POINT('Ctrl Pts',(-12.5818139206897,1.15914512624606,1.81300359108097));
#33577=CARTESIAN_POINT('Ctrl Pts',(-12.470774400677,-0.892822179563889,
1.95792441137325));
#33578=CARTESIAN_POINT('Ctrl Pts',(-12.3597348806643,-2.12890349408833,
0.313638897190672));
#33579=CARTESIAN_POINT('Ctrl Pts',(-12.2486953606516,-1.41953298474134,
-1.61725865284556));
#33580=CARTESIAN_POINT('Ctrl Pts',(-12.1376558406389,0.587046647461331,
-2.07025980946279));
#33581=CARTESIAN_POINT('Ctrl Pts',(-12.0266163206262,2.05716656029549,-0.631399388798012));
#33582=CARTESIAN_POINT('Ctrl Pts',(-11.9155768006135,1.64738987478806,1.38445153234711));
#33583=CARTESIAN_POINT('Ctrl Pts',(-11.8045372806008,-0.267817961278038,
2.13515174743843));
#33584=CARTESIAN_POINT('Ctrl Pts',(-11.6934977605881,-1.93828622005437,
0.934690309203982));
#33585=CARTESIAN_POINT('Ctrl Pts',(-11.5824582405754,-1.83749407531276,
-1.11991739345498));
#33586=CARTESIAN_POINT('Ctrl Pts',(-11.4714187205627,-0.0575482206464092,
-2.15111311819553));
#33587=CARTESIAN_POINT('Ctrl Pts',(-11.36037920055,1.77498681484848,-1.21656124058205));
#33588=CARTESIAN_POINT('Ctrl Pts',(-11.2493396805373,1.98548903115562,0.829718477637558));
#33589=CARTESIAN_POINT('Ctrl Pts',(-11.1383001605246,0.381595589010167,
2.11777814027354));
#33590=CARTESIAN_POINT('Ctrl Pts',(-11.027260640512,-1.57101062319865,1.47055263991789));
#33591=CARTESIAN_POINT('Ctrl Pts',(-10.9162211204993,-2.08798319080583,
-0.520505177577319));
#33592=CARTESIAN_POINT('Ctrl Pts',(-10.8051816004866,-0.696898057326079,
-2.03591074034881));
#33593=CARTESIAN_POINT('Ctrl Pts',(-10.6941420804739,1.33103210010252,-1.69084387022254));
#33594=CARTESIAN_POINT('Ctrl Pts',(-10.5831025604612,2.14262772946706,0.199363632318784));
#33595=CARTESIAN_POINT('Ctrl Pts',(-10.4720630404485,0.99622994309236,1.90738704657934));
#33596=CARTESIAN_POINT('Ctrl Pts',(-10.3610235204358,-1.06055075409358,
1.87238659014746));
#33597=CARTESIAN_POINT('Ctrl Pts',(-10.2499840004231,-2.1481703762994,0.126346663439019));
#33598=CARTESIAN_POINT('Ctrl Pts',(-10.1389444804104,-1.27273155637141,
-1.73515239399567));
#33599=CARTESIAN_POINT('Ctrl Pts',(-10.0279049603977,0.765765116820998,
-2.01102044515529));
#33600=CARTESIAN_POINT('Ctrl Pts',(-9.91686544038503,2.10448411229651,-0.449161514451188));
#33601=CARTESIAN_POINT('Ctrl Pts',(-9.80582592037233,1.52006640103793,1.52315382723088));
#33602=CARTESIAN_POINT('Ctrl Pts',(-9.69478640035963,-0.453430693347546,
2.1035684089905));
#33603=CARTESIAN_POINT('Ctrl Pts',(-9.58374688034695,-2.01257008113814,
0.76168307942353));
#33604=CARTESIAN_POINT('Ctrl Pts',(-9.47270736033426,-1.73256638616727,
-1.2762496474028));
#33605=CARTESIAN_POINT('Ctrl Pts',(-9.36166784032154,0.130705148471866,
-2.1479095905404));
#33606=CARTESIAN_POINT('Ctrl Pts',(-9.25062832030888,1.87453464631127,-1.05674940489747));
#33607=CARTESIAN_POINT('Ctrl Pts',(-9.13958880029616,1.90536171980257,1.00009807603229));
#33608=CARTESIAN_POINT('Ctrl Pts',(-9.02854928028348,0.195015723111051,
2.14302783759613));
#33609=CARTESIAN_POINT('Ctrl Pts',(-8.91750976027079,-1.69354112027386,
1.32759855337147));
#33610=CARTESIAN_POINT('Ctrl Pts',(-8.80647024025808,-2.0344925083683,-0.70102758744985));
#33611=CARTESIAN_POINT('Ctrl Pts',(-8.69543072024542,-0.516267483793617,
-2.08903502367717));
#33612=CARTESIAN_POINT('Ctrl Pts',(-8.58439120023269,1.47373727186836,-1.56802356438877));
#33613=CARTESIAN_POINT('Ctrl Pts',(-8.47335168022003,2.11699950424307,0.385891881240195));
#33614=CARTESIAN_POINT('Ctrl Pts',(-8.36231216020731,0.825688113106338,
1.98716848426282));
#33615=CARTESIAN_POINT('Ctrl Pts',(-8.25127264019463,-1.22016027327337,
1.7725146973997));
#33616=CARTESIAN_POINT('Ctrl Pts',(-8.14023312018193,-2.15099192185977,
-0.0619128182729752));
#33617=CARTESIAN_POINT('Ctrl Pts',(-8.02919360016924,-1.11618672070874,
-1.83976266118376));
#33618=CARTESIAN_POINT('Ctrl Pts',(-7.91815408015655,0.938621264792929,
-1.93638569666557));
#33619=CARTESIAN_POINT('Ctrl Pts',(-7.80711456014386,2.13569076821376,-0.263485080296819));
#33620=CARTESIAN_POINT('Ctrl Pts',(-7.69607504013116,1.38110604598068,1.65019560498993));
#33621=CARTESIAN_POINT('Ctrl Pts',(-7.58503552011847,-0.635572182874023,
2.05588118463331));
#33622=CARTESIAN_POINT('Ctrl Pts',(-7.47399600010578,-2.07144669478819,
0.582844778327466));
#33623=CARTESIAN_POINT('Ctrl Pts',(-7.36295648009308,-1.61437502026476,
-1.42281156128196));
#33624=CARTESIAN_POINT('Ctrl Pts',(-7.25191696008039,0.317957903210428,
-2.12826272268217));
#33625=CARTESIAN_POINT('Ctrl Pts',(-7.1408774400677,1.9597319617898,-0.888847615124196));
#33626=CARTESIAN_POINT('Ctrl Pts',(-7.029837920055,1.81064789554103,1.16282141506997));
#33627=CARTESIAN_POINT('Ctrl Pts',(-6.91879840004231,0.00694291267913799,
2.15187156701696));
#33628=CARTESIAN_POINT('Ctrl Pts',(-6.80775888002961,-1.80310669884822,
1.17448102476845));
#33629=CARTESIAN_POINT('Ctrl Pts',(-6.69671936001694,-1.96542675116825,
-0.876183274643305));
#33630=CARTESIAN_POINT('Ctrl Pts',(-6.58567984000421,-0.331684620132549,
-2.12616668155156));
#33631=CARTESIAN_POINT('Ctrl Pts',(-6.47464031999155,1.60516023537086,-1.43319924077452));
#33632=CARTESIAN_POINT('Ctrl Pts',(-6.36360079997884,2.07516457124545,0.569465931571117));
#33633=CARTESIAN_POINT('Ctrl Pts',(-6.25256127996616,0.648825220723096,
2.05173713665423));
#33634=CARTESIAN_POINT('Ctrl Pts',(-6.14152175995345,-1.37042884506684,
1.65907330325736));
#33635=CARTESIAN_POINT('Ctrl Pts',(-6.03048223994078,-2.13734653040332,
-0.249698325876242));
#33636=CARTESIAN_POINT('Ctrl Pts',(-5.91944271992806,-0.951096908078864,
-1.93028860961653));
#33637=CARTESIAN_POINT('Ctrl Pts',(-5.80840319991538,1.10429178966098,-1.84692693094769));
#33638=CARTESIAN_POINT('Ctrl Pts',(-5.69736367990268,2.15054762522653,-0.0757915338613339));
#33639=CARTESIAN_POINT('Ctrl Pts',(-5.58632415989,1.23157262180047,1.76460429621033));
#33640=CARTESIAN_POINT('Ctrl Pts',(-5.47528463987729,-0.812848044129805,
1.99245514431989));
#33641=CARTESIAN_POINT('Ctrl Pts',(-5.36424511986461,-2.11446533058618,
0.399544504056276));
#33642=CARTESIAN_POINT('Ctrl Pts',(-5.25320559985191,-1.48382479261571,
-1.55848112910982));
#33643=CARTESIAN_POINT('Ctrl Pts',(-5.14216607983922,0.502776528507167,
-2.09232292138541));
#33644=CARTESIAN_POINT('Ctrl Pts',(-5.03112655982653,2.02992653250826,-0.714141244846878));
#33645=CARTESIAN_POINT('Ctrl Pts',(-4.92008703981383,1.70207264086103,1.31664276483973));
#33646=CARTESIAN_POINT('Ctrl Pts',(-4.80904751980114,-0.181183049280004,
2.14424162528995));
#33647=CARTESIAN_POINT('Ctrl Pts',(-4.69800799978845,-1.89886857869975,
1.012372246656));
#33648=CARTESIAN_POINT('Ctrl Pts',(-4.58696847977575,-1.88131465269946,
-1.04463133329937));
#33649=CARTESIAN_POINT('Ctrl Pts',(-4.47592895976307,-0.144562542031095,
-2.14702145224819));
#33650=CARTESIAN_POINT('Ctrl Pts',(-4.36488943975037,1.72429488099121,-1.28740304813998));
#33651=CARTESIAN_POINT('Ctrl Pts',(-4.25384991973768,2.0174431981608,0.748680430602484));
#33652=CARTESIAN_POINT('Ctrl Pts',(-4.14281039972499,0.466995241324839,
2.10059869788404));
#33653=CARTESIAN_POINT('Ctrl Pts',(-4.03177087971229,-1.51020608714031,
1.53293085928163));
#33654=CARTESIAN_POINT('Ctrl Pts',(-3.9207313596996,-2.10733866434047,-0.435572265814925));
#33655=CARTESIAN_POINT('Ctrl Pts',(-3.8096918396869,-0.778725964952054,
-2.00603721712242));
#33656=CARTESIAN_POINT('Ctrl Pts',(-3.69865231967421,1.26150839930913,-1.74332900034742));
#33657=CARTESIAN_POINT('Ctrl Pts',(-3.58761279966152,2.14894094653692,0.112482235310861));
#33658=CARTESIAN_POINT('Ctrl Pts',(-3.47657327964882,1.07261088290665,1.86550404417541));
#33659=CARTESIAN_POINT('Ctrl Pts',(-3.36553375963613,-0.983901140254003,
1.9137758466519));
#33660=CARTESIAN_POINT('Ctrl Pts',(-3.25449423962344,-2.14129665898335,
0.213185513407649));
#33661=CARTESIAN_POINT('Ctrl Pts',(-3.14345471961075,-1.34191513163117,
-1.68221973132061));
#33662=CARTESIAN_POINT('Ctrl Pts',(-3.03241519959805,0.683746143853823,
-2.04036532416529));
#33663=CARTESIAN_POINT('Ctrl Pts',(-2.92137567958536,2.08458098322634,-0.533967760061011));
#33664=CARTESIAN_POINT('Ctrl Pts',(-2.81033615957267,1.58046715475138,1.46038454446989));
#33665=CARTESIAN_POINT('Ctrl Pts',(-2.69929663955997,-0.367921963239354,
2.12019642390948));
#33666=CARTESIAN_POINT('Ctrl Pts',(-2.58825711954728,-1.98009365321621,
0.842513243387684));
#33667=CARTESIAN_POINT('Ctrl Pts',(-2.47721759953459,-1.78280013522666,
-1.20508220638155));
#33668=CARTESIAN_POINT('Ctrl Pts',(-2.36617807952189,0.0436662384648719,
-2.15143968471892));
#33669=CARTESIAN_POINT('Ctrl Pts',(-2.2551385595092,1.83022916744761,-1.1317511251033));
#33670=CARTESIAN_POINT('Ctrl Pts',(-2.14409903949651,1.94427728093947,0.9221633899726));
#33671=CARTESIAN_POINT('Ctrl Pts',(-2.03305951948381,0.281590157821288,
2.13337912732726));
#33672=CARTESIAN_POINT('Ctrl Pts',(-1.92201999947113,-1.6384218992803,1.39505301297495));
#33673=CARTESIAN_POINT('Ctrl Pts',(-1.81098047945843,-2.06119811449319,
-0.61811160805078));
#33674=CARTESIAN_POINT('Ctrl Pts',(-1.69994095944574,-0.600393354215775,
-2.06642872374214));
#33675=CARTESIAN_POINT('Ctrl Pts',(-1.58890143943304,1.40906728405564,-1.62638474445002));
#33676=CARTESIAN_POINT('Ctrl Pts',(-1.47786191942035,2.13088348224722,0.299894410085385));
#33677=CARTESIAN_POINT('Ctrl Pts',(-1.36682239940766,0.905436905709838,
1.95212333414178));
#33678=CARTESIAN_POINT('Ctrl Pts',(-1.25578287939496,-1.14742034303764,
1.82044386326689));
#33679=CARTESIAN_POINT('Ctrl Pts',(-1.14474335938227,-2.15173837355173,
0.0251978250021854));
#33680=CARTESIAN_POINT('Ctrl Pts',(-1.03370383936958,-1.18972652745971,
-1.79308645214156));
#33681=CARTESIAN_POINT('Ctrl Pts',(-0.922664319356884,0.859470107733127,
-1.97277557969645));
#33682=CARTESIAN_POINT('Ctrl Pts',(-0.811624799344192,2.12329826860884,
-0.349729528680995));
#33683=CARTESIAN_POINT('Ctrl Pts',(-0.700585279331502,1.44672174184939,
1.59299019289389));
#33684=CARTESIAN_POINT('Ctrl Pts',(-0.589545759318803,-0.55176690423342,
2.07983659183781));
#33685=CARTESIAN_POINT('Ctrl Pts',(-0.478506239306111,-2.04630728936339,
0.66636318757467));
#33686=CARTESIAN_POINT('Ctrl Pts',(-0.367466719293421,-1.67035713710672,
-1.35661003079366));
#33687=CARTESIAN_POINT('Ctrl Pts',(-0.256427199280725,0.231025933890705,
-2.13880958007493));
#33688=CARTESIAN_POINT('Ctrl Pts',(-0.145387679268034,1.92318326618488,
-0.968555914648296));
#33689=CARTESIAN_POINT('Ctrl Pts',(-0.0343481592553421,1.85414808526718,
1.09089988066647));
#33690=CARTESIAN_POINT('Ctrl Pts',(0.0396781874197904,0.684045639651843,
1.79298893531071));
#33691=CARTESIAN_POINT('Ctrl Pts',(0.0766913607573549,0.0795783122554267,
1.81942719557457));
#33692=CARTESIAN_POINT('Ctrl Pts',(-19.7226913607574,0.980771099081406,
-1.37424797458504));
#33693=CARTESIAN_POINT('Ctrl Pts',(-19.6856781874198,1.43733677117747,-1.04840691510689));
#33694=CARTESIAN_POINT('Ctrl Pts',(-19.6116518407446,1.99239321049778,0.0883666108304189));
#33695=CARTESIAN_POINT('Ctrl Pts',(-19.500612320732,1.00592855143894,1.72427260675583));
#33696=CARTESIAN_POINT('Ctrl Pts',(-19.3895728007192,-0.900609403940542,
1.77941017743441));
#33697=CARTESIAN_POINT('Ctrl Pts',(-19.2785332807066,-1.98371002846714,
0.211022941123868));
#33698=CARTESIAN_POINT('Ctrl Pts',(-19.1674937606938,-1.25426946634223,
-1.55152933282018));
#33699=CARTESIAN_POINT('Ctrl Pts',(-19.0564542406812,0.621478012272129,
-1.89555506074211));
#33700=CARTESIAN_POINT('Ctrl Pts',(-18.9454147206685,1.92923822913921,-0.507734630855354));
#33701=CARTESIAN_POINT('Ctrl Pts',(-18.8343752006558,1.4740395628997,1.34425993980917));
#33702=CARTESIAN_POINT('Ctrl Pts',(-18.7233356806431,-0.328195323543107,
1.96773112193963));
#33703=CARTESIAN_POINT('Ctrl Pts',(-18.6122961606304,-1.83050692923332,
0.793087344565633));
#33704=CARTESIAN_POINT('Ctrl Pts',(-18.5012566406177,-1.66005469660814,
-1.10632979622673));
#33705=CARTESIAN_POINT('Ctrl Pts',(-18.390217120605,0.0274046903966734,
-1.99473704181564));
#33706=CARTESIAN_POINT('Ctrl Pts',(-18.2791776005923,1.68981956971848,-1.06030523397109));
#33707=CARTESIAN_POINT('Ctrl Pts',(-18.1681380805796,1.80803055107265,0.843067330871544));
#33708=CARTESIAN_POINT('Ctrl Pts',(-18.0570985605669,0.274012050901109,
1.97601915702686));
#33709=CARTESIAN_POINT('Ctrl Pts',(-17.9460590405543,-1.51040616636786,
1.30323027908932));
#33710=CARTESIAN_POINT('Ctrl Pts',(-17.8350195205416,-1.91457289594923,
-0.56048762900514));
#33711=CARTESIAN_POINT('Ctrl Pts',(-17.7239800005289,-0.569149070404872,
-1.91201588634746));
#33712=CARTESIAN_POINT('Ctrl Pts',(-17.6129404805162,1.29637913770427,-1.51629047136732));
#33713=CARTESIAN_POINT('Ctrl Pts',(-17.5019009605035,1.9772396831027,0.265063861366327));
#33714=CARTESIAN_POINT('Ctrl Pts',(-17.3908614404908,0.851243048311522,
1.80419534588497));
#33715=CARTESIAN_POINT('Ctrl Pts',(-17.2798219204781,-1.05264339539859,
1.69460245849397));
#33716=CARTESIAN_POINT('Ctrl Pts',(-17.1687824004654,-1.99459473280011,
0.0364342227546489));
#33717=CARTESIAN_POINT('Ctrl Pts',(-17.0577428804527,-1.11382936463886,
-1.65502862284421));
#33718=CARTESIAN_POINT('Ctrl Pts',(-16.9467033604401,0.784784569075727,
-1.83407981872));
#33719=CARTESIAN_POINT('Ctrl Pts',(-16.8356638404273,1.96624031556741,-0.337097346471846));
#33720=CARTESIAN_POINT('Ctrl Pts',(-16.7246243204147,1.35089042053518,1.4679341506979));
#33721=CARTESIAN_POINT('Ctrl Pts',(-16.6135848004019,-0.498941093600838,
1.93152618023922));
#33722=CARTESIAN_POINT('Ctrl Pts',(-16.5025452803893,-1.89282621883312,
0.630035320306451));
#33723=CARTESIAN_POINT('Ctrl Pts',(-16.3915057603766,-1.55699356682629,
-1.24719951585892));
#33724=CARTESIAN_POINT('Ctrl Pts',(-16.2804662403639,0.201663549851218,
-1.98470839476804));
#33725=CARTESIAN_POINT('Ctrl Pts',(-16.1694267203512,1.77603484899781,-0.908534982649458));
#33726=CARTESIAN_POINT('Ctrl Pts',(-16.0583872003385,1.72741560590332,0.99788322164133));
#33727=CARTESIAN_POINT('Ctrl Pts',(-15.9473476803258,0.100235450857364,
1.99240770274486));
#33728=CARTESIAN_POINT('Ctrl Pts',(-15.8363081603131,-1.61854267527115,
1.16621404891383));
#33729=CARTESIAN_POINT('Ctrl Pts',(-15.7252686403004,-1.8582510322134,-0.725698767283147));
#33730=CARTESIAN_POINT('Ctrl Pts',(-15.6142291202877,-0.399837388854213,
-1.95444766162579));
#33731=CARTESIAN_POINT('Ctrl Pts',(-15.503189600275,1.42395889376444,-1.39716737309035));
#33732=CARTESIAN_POINT('Ctrl Pts',(-15.3921500802623,1.94650153351731,0.436883714017789));
#33733=CARTESIAN_POINT('Ctrl Pts',(-15.2811105602496,0.690276385502817,
1.87169818912575));
#33734=CARTESIAN_POINT('Ctrl Pts',(-15.1700710402369,-1.19674271671436,
1.59610227415113));
#33735=CARTESIAN_POINT('Ctrl Pts',(-15.0590315202242,-1.99014470223182,
-0.138056741008676));
#33736=CARTESIAN_POINT('Ctrl Pts',(-14.9479920002116,-0.964896546267425,
-1.74605562756762));
#33737=CARTESIAN_POINT('Ctrl Pts',(-14.8369524801988,0.942101182186204,
-1.75845982669002));
#33738=CARTESIAN_POINT('Ctrl Pts',(-14.7259129601862,1.98818038227767,-0.163934032725192));
#33739=CARTESIAN_POINT('Ctrl Pts',(-14.6148734401735,1.21740449164842,1.58039928602666));
#33740=CARTESIAN_POINT('Ctrl Pts',(-14.5038339201608,-0.665869826102309,
1.88051933631266));
#33741=CARTESIAN_POINT('Ctrl Pts',(-14.3927944001481,-1.94065358932632,
0.462167984389029));
#33742=CARTESIAN_POINT('Ctrl Pts',(-14.2817548801354,-1.44201358048108,
-1.37852545615505));
#33743=CARTESIAN_POINT('Ctrl Pts',(-14.1707153601227,0.374378951193126,
-1.95948360556114));
#33744=CARTESIAN_POINT('Ctrl Pts',(-14.05967584011,1.84865347919068,-0.749810585038333));
#33745=CARTESIAN_POINT('Ctrl Pts',(-13.9486363200973,1.63357652047938,1.14506041382008));
#33746=CARTESIAN_POINT('Ctrl Pts',(-13.8375968000846,-0.0743085575408296,
1.99354303636404));
#33747=CARTESIAN_POINT('Ctrl Pts',(-13.7265572800719,-1.71428838800121,
1.02027002422082));
#33748=CARTESIAN_POINT('Ctrl Pts',(-13.6155177600592,-1.78770332703292,
-0.885354400268458));
#33749=CARTESIAN_POINT('Ctrl Pts',(-13.5044782400465,-0.227464740775772,
-1.98191709999766));
#33750=CARTESIAN_POINT('Ctrl Pts',(-13.3934387200338,1.54063751616327,-1.26734827231887));
#33751=CARTESIAN_POINT('Ctrl Pts',(-13.2823992000211,1.9008619270339,0.605359012415223));
#33752=CARTESIAN_POINT('Ctrl Pts',(-13.1713596800085,0.524025304774173,
1.92487222420494));
#33753=CARTESIAN_POINT('Ctrl Pts',(-13.0603201599958,-1.33168036333877,
1.48538311874655));
#33754=CARTESIAN_POINT('Ctrl Pts',(-12.9492806399831,-1.97045910222959,
-0.311490812063336));
#33755=CARTESIAN_POINT('Ctrl Pts',(-12.8382411199704,-0.808576953982255,
-1.82371568755882));
#33756=CARTESIAN_POINT('Ctrl Pts',(-12.7272015999577,1.09220553156706,-1.66937793095921));
#33757=CARTESIAN_POINT('Ctrl Pts',(-12.616162079945,1.99489991714847,0.0104842796768135));
#33758=CARTESIAN_POINT('Ctrl Pts',(-12.5051225599323,1.0745987122607,1.68076566099114));
#33759=CARTESIAN_POINT('Ctrl Pts',(-12.3940830399196,-0.827700986453924,
1.81511616063064));
#33760=CARTESIAN_POINT('Ctrl Pts',(-12.2830435199069,-1.97362426970941,
0.290762517483453));
#33761=CARTESIAN_POINT('Ctrl Pts',(-12.1720039998942,-1.31599424685915,
-1.49929808303518));
#33762=CARTESIAN_POINT('Ctrl Pts',(-12.0609644798815,0.544228291276939,
-1.91925797289815));
#33763=CARTESIAN_POINT('Ctrl Pts',(-11.9499249598688,1.90711972689606,-0.585346006088044));
#33764=CARTESIAN_POINT('Ctrl Pts',(-11.8388854398562,1.52723157605959,1.28347158622459));
#33765=CARTESIAN_POINT('Ctrl Pts',(-11.7278459198434,-0.248283696142248,
1.97941678425471));
#33766=CARTESIAN_POINT('Ctrl Pts',(-11.6168063998308,-1.79691035134536,
0.866515313648441));
#33767=CARTESIAN_POINT('Ctrl Pts',(-11.505766879818,-1.70346984377399,-1.03823219508546));
#33768=CARTESIAN_POINT('Ctrl Pts',(-11.3947273598054,-0.0533507344329003,
-1.99421395509479));
#33769=CARTESIAN_POINT('Ctrl Pts',(-11.2836878397927,1.64552177490757,-1.12782697603151));
#33770=CARTESIAN_POINT('Ctrl Pts',(-11.17264831978,1.84067025584392,0.76919997972621));
#33771=CARTESIAN_POINT('Ctrl Pts',(-11.0616087997673,0.353762543852217,
1.96331038354269));
#33772=CARTESIAN_POINT('Ctrl Pts',(-10.9505692797546,-1.45642331957557,
1.36329260019844));
#33773=CARTESIAN_POINT('Ctrl Pts',(-10.8395297597419,-1.93568863575209,
-0.48254026254764));
#33774=CARTESIAN_POINT('Ctrl Pts',(-10.7284902397292,-0.646067293924532,
-1.88741427653824));
#33775=CARTESIAN_POINT('Ctrl Pts',(-10.6174507197165,1.23394849217886,-1.56751609822957));
#33776=CARTESIAN_POINT('Ctrl Pts',(-10.5064111997038,1.98634747867679,0.184822329586263));
#33777=CARTESIAN_POINT('Ctrl Pts',(-10.3953716796911,0.923566333259427,
1.76826492009231));
#33778=CARTESIAN_POINT('Ctrl Pts',(-10.2843321596784,-0.983195674839188,
1.73581734768865));
#33779=CARTESIAN_POINT('Ctrl Pts',(-10.1732926396658,-1.99148585265059,
0.117131115643584));
#33780=CARTESIAN_POINT('Ctrl Pts',(-10.0622531196531,-1.17990030804818,
-1.60859282064391));
#33781=CARTESIAN_POINT('Ctrl Pts',(-9.95121359964037,0.709911287031804,
-1.8643394444425));
#33782=CARTESIAN_POINT('Ctrl Pts',(-9.84017407962766,1.95098600325465,-0.416400305792137));
#33783=CARTESIAN_POINT('Ctrl Pts',(-9.72913455961498,1.40919489727413,1.41205713094616));
#33784=CARTESIAN_POINT('Ctrl Pts',(-9.61809503960227,-0.420358096788729,
1.95013709005892));
#33785=CARTESIAN_POINT('Ctrl Pts',(-9.50705551958959,-1.86577605215789,
0.706126987696579));
#33786=CARTESIAN_POINT('Ctrl Pts',(-9.3960159995769,-1.60619543258667,-1.18316179447151));
#33787=CARTESIAN_POINT('Ctrl Pts',(-9.28497647956421,0.12117169891277,-1.99124408823779));
#33788=CARTESIAN_POINT('Ctrl Pts',(-9.17393695955151,1.73780872765929,-0.979671590702989));
#33789=CARTESIAN_POINT('Ctrl Pts',(-9.06289743953882,1.76638731779995,0.927152330027173));
#33790=CARTESIAN_POINT('Ctrl Pts',(-8.95185791952612,0.180791550756394,
1.98671840348209));
#33791=CARTESIAN_POINT('Ctrl Pts',(-8.84081839951343,-1.57001661465857,
1.23076538351361));
#33792=CARTESIAN_POINT('Ctrl Pts',(-8.72977887950074,-1.88609948840221,
-0.649895621933452));
#33793=CARTESIAN_POINT('Ctrl Pts',(-8.61873935948805,-0.478611660183903,
-1.93666374941427));
#33794=CARTESIAN_POINT('Ctrl Pts',(-8.50769983947534,1.36624494957686,-1.45365413263095));
#33795=CARTESIAN_POINT('Ctrl Pts',(-8.39666031946266,1.96258854012834,0.357745470574083));
#33796=CARTESIAN_POINT('Ctrl Pts',(-8.28562079944997,0.765463584311097,
1.84222721200533));
#33797=CARTESIAN_POINT('Ctrl Pts',(-8.17458127943727,-1.13116350034402,
1.64322997022596));
#33798=CARTESIAN_POINT('Ctrl Pts',(-8.06354175942458,-1.99410159864917,
-0.0573969844518235));
#33799=CARTESIAN_POINT('Ctrl Pts',(-7.95250223941189,-1.03477363235835,
-1.70557296218463));
#33800=CARTESIAN_POINT('Ctrl Pts',(-7.84146271939919,0.87015955086961,-1.79514844945752));
#33801=CARTESIAN_POINT('Ctrl Pts',(-7.7304231993865,1.97991648961337,-0.244266849401202));
#33802=CARTESIAN_POINT('Ctrl Pts',(-7.61938367937381,1.2803701149249,1.52983266024965));
#33803=CARTESIAN_POINT('Ctrl Pts',(-7.50834415936111,-0.589214442437421,
1.90592810472549));
#33804=CARTESIAN_POINT('Ctrl Pts',(-7.39730463934842,-1.92035828847847,
0.540332900563502));
#33805=CARTESIAN_POINT('Ctrl Pts',(-7.28626511933573,-1.49662477855607,
-1.31903368864154));
#33806=CARTESIAN_POINT('Ctrl Pts',(-7.17522559932303,0.294766501283195,
-1.97303023526772));
#33807=CARTESIAN_POINT('Ctrl Pts',(-7.06418607931034,1.81679187086397,-0.8240163211502));
#33808=CARTESIAN_POINT('Ctrl Pts',(-6.95314655929765,1.6785817865682,1.07800685775223));
#33809=CARTESIAN_POINT('Ctrl Pts',(-6.84210703928495,0.00643650640064556,
1.99491708372672));
#33810=CARTESIAN_POINT('Ctrl Pts',(-6.73106751927226,-1.67159063414775,
1.0888160319305));
#33811=CARTESIAN_POINT('Ctrl Pts',(-6.62002799925957,-1.82207129032072,
-0.812275699838614));
#33812=CARTESIAN_POINT('Ctrl Pts',(-6.50898847924688,-0.307492010793712,
-1.97108707642695));
#33813=CARTESIAN_POINT('Ctrl Pts',(-6.39794895923418,1.48808210710229,-1.32866370541284));
#33814=CARTESIAN_POINT('Ctrl Pts',(-6.28690943922149,1.92380498825995,0.527929888058504));
#33815=CARTESIAN_POINT('Ctrl Pts',(-6.1758699192088,0.601500822359763,1.90208631777315));
#33816=CARTESIAN_POINT('Ctrl Pts',(-6.0648303991961,-1.27047169401729,1.53806283170103));
#33817=CARTESIAN_POINT('Ctrl Pts',(-5.95379087918341,-1.98145148283935,
-0.231485681442862));
#33818=CARTESIAN_POINT('Ctrl Pts',(-5.84275135917072,-0.881725238294048,
-1.78949607535603));
#33819=CARTESIAN_POINT('Ctrl Pts',(-5.73171183915802,1.0237463008388,-1.71221468019586));
#33820=CARTESIAN_POINT('Ctrl Pts',(-5.62067231914534,1.993689708387,-0.0702634060598052));
#33821=CARTESIAN_POINT('Ctrl Pts',(-5.50963279913263,1.14174344823272,1.63589654256526));
#33822=CARTESIAN_POINT('Ctrl Pts',(-5.39859327911995,-0.753560051892996,
1.84712827051895));
#33823=CARTESIAN_POINT('Ctrl Pts',(-5.28755375910725,-1.96023920553107,
0.370402290298364));
#33824=CARTESIAN_POINT('Ctrl Pts',(-5.17651423909456,-1.37559670075934,
-1.44480770915003));
#33825=CARTESIAN_POINT('Ctrl Pts',(-5.06547471908186,0.466104716187191,
-1.93971183249147));
#33826=CARTESIAN_POINT('Ctrl Pts',(-4.95443519906918,1.88186654839468,-0.662052787617739));
#33827=CARTESIAN_POINT('Ctrl Pts',(-4.84339567905647,1.57792585814243,1.22060869477682));
#33828=CARTESIAN_POINT('Ctrl Pts',(-4.73235615904379,-0.16796781268475,
1.98784365920996));
#33829=CARTESIAN_POINT('Ctrl Pts',(-4.62131663903109,-1.76036777726992,
0.938531239921795));
#33830=CARTESIAN_POINT('Ctrl Pts',(-4.5102771190184,-1.74409420992455,-0.968437394190764));
#33831=CARTESIAN_POINT('Ctrl Pts',(-4.39923759900571,-0.134018353690417,
-1.99042072950253));
#33832=CARTESIAN_POINT('Ctrl Pts',(-4.28819807899301,1.59852723935581,-1.19350168185761));
#33833=CARTESIAN_POINT('Ctrl Pts',(-4.17715855898033,1.87029373088395,0.694072733778989));
#33834=CARTESIAN_POINT('Ctrl Pts',(-4.06611903896762,0.432933265729,1.94738398550062));
#33835=CARTESIAN_POINT('Ctrl Pts',(-3.95507951895494,-1.40005378079356,
1.42112104004054));
#33836=CARTESIAN_POINT('Ctrl Pts',(-3.84403999894224,-1.95363234829038,
-0.403802237824197));
#33837=CARTESIAN_POINT('Ctrl Pts',(-3.73300047892955,-0.721926789142902,
-1.85971968604833));
#33838=CARTESIAN_POINT('Ctrl Pts',(-3.62196095891686,1.16949575226516,-1.61617303683714));
#33839=CARTESIAN_POINT('Ctrl Pts',(-3.51092143890416,1.99220021857957,0.104277939388565));
#33840=CARTESIAN_POINT('Ctrl Pts',(-3.39988191889147,0.99437615483157,1.72943680493244));
#33841=CARTESIAN_POINT('Ctrl Pts',(-3.28884239887877,-0.912136775947003,
1.77418773007997));
#33842=CARTESIAN_POINT('Ctrl Pts',(-3.17780287886609,-1.98511349460065,
0.197636062123149));
#33843=CARTESIAN_POINT('Ctrl Pts',(-3.06676335885339,-1.24403773070594,
-1.55952099188045));
#33844=CARTESIAN_POINT('Ctrl Pts',(-2.95572383884069,0.633874662509295,
-1.89154394928109));
#33845=CARTESIAN_POINT('Ctrl Pts',(-2.84468431882801,1.93253458040476,-0.495020903213892));
#33846=CARTESIAN_POINT('Ctrl Pts',(-2.73364479881531,1.46519010502714,1.35386615132057));
#33847=CARTESIAN_POINT('Ctrl Pts',(-2.62260527880262,-0.341086253099156,
1.96555228097401));
#33848=CARTESIAN_POINT('Ctrl Pts',(-2.51156575878993,-1.83566840917728,
0.781061513271475));
#33849=CARTESIAN_POINT('Ctrl Pts',(-2.40052623877724,-1.65276520269481,
-1.11718520642857));
#33850=CARTESIAN_POINT('Ctrl Pts',(-2.28948671876454,0.0404812844924485,
-1.99451670231561));
#33851=CARTESIAN_POINT('Ctrl Pts',(-2.17844719875185,1.69673482806298,-1.04920279100363));
#33852=CARTESIAN_POINT('Ctrl Pts',(-2.06740767873915,1.80246443268206,0.854902090273845));
#33853=CARTESIAN_POINT('Ctrl Pts',(-1.95636815872646,0.261051368054344,
1.97777345655945));
#33854=CARTESIAN_POINT('Ctrl Pts',(-1.84532863871377,-1.51891771206272,
1.29329980977728));
#33855=CARTESIAN_POINT('Ctrl Pts',(-1.73428911870107,-1.91085722520509,
-0.573027417365632));
#33856=CARTESIAN_POINT('Ctrl Pts',(-1.62324959868838,-0.556601508026538,
-1.91570632117762));
#33857=CARTESIAN_POINT('Ctrl Pts',(-1.51221007867569,1.30629189965073,-1.50775853036321));
#33858=CARTESIAN_POINT('Ctrl Pts',(-1.401170558663,1.97545984031888,0.278020533921918));
#33859=CARTESIAN_POINT('Ctrl Pts',(-1.2901310386503,0.83939561223033,1.80973820580727));
#33860=CARTESIAN_POINT('Ctrl Pts',(-1.17909151863761,-1.06372911823659,
1.68766325019619));
#33861=CARTESIAN_POINT('Ctrl Pts',(-1.06805199862492,-1.99479360520537,
0.0233599311130506));
#33862=CARTESIAN_POINT('Ctrl Pts',(-0.957012478612224,-1.10294954911385,
-1.66230125013214));
#33863=CARTESIAN_POINT('Ctrl Pts',(-0.845972958599527,0.796781567798704,
-1.82888410563971));
#33864=CARTESIAN_POINT('Ctrl Pts',(-0.734933438586838,1.96842788148691,
-0.324220749111252));
#33865=CARTESIAN_POINT('Ctrl Pts',(-0.623893918574146,1.34119989429253,
1.47679973039398));
#33866=CARTESIAN_POINT('Ctrl Pts',(-0.51285439856145,-0.511521802863037,
1.92813623824627));
#33867=CARTESIAN_POINT('Ctrl Pts',(-0.401814878548755,-1.89705251590108,
0.61775959459427));
#33868=CARTESIAN_POINT('Ctrl Pts',(-0.290775358536067,-1.54852363859167,
-1.2576608046069));
#33869=CARTESIAN_POINT('Ctrl Pts',(-0.17973583852337,0.214175227446937,
-1.98280781972719));
#33870=CARTESIAN_POINT('Ctrl Pts',(-0.0686963185106793,1.78290898567335,
-0.897910809498253));
#33871=CARTESIAN_POINT('Ctrl Pts',(0.0423432015020128,1.71890913368323,
1.01133117883693));
#33872=CARTESIAN_POINT('Ctrl Pts',(0.116369548177145,0.634152313505382,
1.66221084604168));
#33873=CARTESIAN_POINT('Ctrl Pts',(0.15338272151471,0.0737739821678063,
1.68672073681435));
#33874=CARTESIAN_POINT('Ctrl Pts',(-19.646,0.903606778650211,-1.26612599672283));
#33875=CARTESIAN_POINT('Ctrl Pts',(-19.6089868266624,1.32425114367218,-0.965921198291487));
#33876=CARTESIAN_POINT('Ctrl Pts',(-19.5349604799873,1.83563729847737,0.081414173630813));
#33877=CARTESIAN_POINT('Ctrl Pts',(-19.4239209599746,0.926784913186551,
1.58861167214729));
#33878=CARTESIAN_POINT('Ctrl Pts',(-19.3128814399619,-0.829751980945401,
1.63941117334604));
#33879=CARTESIAN_POINT('Ctrl Pts',(-19.2018419199493,-1.82763728486514,
0.194420247730427));
#33880=CARTESIAN_POINT('Ctrl Pts',(-19.0908023999365,-1.15558706114236,
-1.42945935470984));
#33881=CARTESIAN_POINT('Ctrl Pts',(-18.9797628799239,0.572581864613586,
-1.74641810285352));
#33882=CARTESIAN_POINT('Ctrl Pts',(-18.8687233599111,1.7774511739937,-0.467787493561026));
#33883=CARTESIAN_POINT('Ctrl Pts',(-18.7576838398985,1.35806626263998,1.23849733645003));
#33884=CARTESIAN_POINT('Ctrl Pts',(-18.6466443198858,-0.302373835599965,
1.81291555390549));
#33885=CARTESIAN_POINT('Ctrl Pts',(-18.5356047998731,-1.68648777596589,
0.730689455758268));
#33886=CARTESIAN_POINT('Ctrl Pts',(-18.4245652798604,-1.52944624713167,
-1.0192868695147));
#33887=CARTESIAN_POINT('Ctrl Pts',(-18.3135257598477,0.0252485661867687,
-1.83779672371819));
#33888=CARTESIAN_POINT('Ctrl Pts',(-18.202486239835,1.5568693034731,-0.976883390785028));
#33889=CARTESIAN_POINT('Ctrl Pts',(-18.0914467198223,1.66577977622518,0.776737156863176));
#33890=CARTESIAN_POINT('Ctrl Pts',(-17.9804071998096,0.252453550943756,
1.820551509628));
#33891=CARTESIAN_POINT('Ctrl Pts',(-17.8693676797969,-1.39157164370297,
1.20069577440679));
#33892=CARTESIAN_POINT('Ctrl Pts',(-17.7583281597842,-1.76393966810407,
-0.516390033712223));
#33893=CARTESIAN_POINT('Ctrl Pts',(-17.6472886397715,-0.524370017185474,
-1.76158383684904));
#33894=CARTESIAN_POINT('Ctrl Pts',(-17.5362491197588,1.19438366161834,-1.39699298808207));
#33895=CARTESIAN_POINT('Ctrl Pts',(-17.4252095997461,1.821676008134,0.244209379874806));
#33896=CARTESIAN_POINT('Ctrl Pts',(-17.3141700797334,0.784269631776072,
1.66224631422945));
#33897=CARTESIAN_POINT('Ctrl Pts',(-17.2031305597208,-0.96982436419101,
1.56127588796884));
#33898=CARTESIAN_POINT('Ctrl Pts',(-17.0920910397081,-1.83766561117703,
0.0335676802536325));
#33899=CARTESIAN_POINT('Ctrl Pts',(-16.9810515196953,-1.02619639290964,
-1.5248156107606));
#33900=CARTESIAN_POINT('Ctrl Pts',(-16.8700119996827,0.723039919366596,
-1.68977956052457));
#33901=CARTESIAN_POINT('Ctrl Pts',(-16.7589724796699,1.81154203999908,-0.310575472322002));
#33902=CARTESIAN_POINT('Ctrl Pts',(-16.6479329596573,1.24460614954145,1.35244120715334));
#33903=CARTESIAN_POINT('Ctrl Pts',(-16.5368934396446,-0.459685807164506,
1.77955911551557));
#33904=CARTESIAN_POINT('Ctrl Pts',(-16.4258539196319,-1.74390395857547,
0.58046590764267));
#33905=CARTESIAN_POINT('Ctrl Pts',(-16.3148143996192,-1.43449367810364,
-1.14907335454206));
#33906=CARTESIAN_POINT('Ctrl Pts',(-16.2037748796065,0.185797227123519,
-1.82855710250446));
#33907=CARTESIAN_POINT('Ctrl Pts',(-16.0927353595938,1.63630140628791,-0.837053997341315));
#33908=CARTESIAN_POINT('Ctrl Pts',(-15.9816958395811,1.59150738893344,0.919372567381872));
#33909=CARTESIAN_POINT('Ctrl Pts',(-15.8706563195684,0.0923492065994037,
1.83565065051508));
#33910=CARTESIAN_POINT('Ctrl Pts',(-15.7596167995557,-1.49120027525227,
1.07445959708913));
#33911=CARTESIAN_POINT('Ctrl Pts',(-15.648577279543,-1.7120490507056,-0.668602822808828));
#33912=CARTESIAN_POINT('Ctrl Pts',(-15.5375377595304,-0.368379304064812,
-1.80067719900824));
#33913=CARTESIAN_POINT('Ctrl Pts',(-15.4264982395177,1.31192580014841,-1.28724216120951));
#33914=CARTESIAN_POINT('Ctrl Pts',(-15.315458719505,1.79335624998195,0.402510928225848));
#33915=CARTESIAN_POINT('Ctrl Pts',(-15.2044191994923,0.635967374718456,
1.72443822301191));
#33916=CARTESIAN_POINT('Ctrl Pts',(-15.0933796794796,-1.10258635489586,
1.47052542197953));
#33917=CARTESIAN_POINT('Ctrl Pts',(-14.9823401594669,-1.83356569653797,
-0.127194823675595));
#33918=CARTESIAN_POINT('Ctrl Pts',(-14.8713006394542,-0.888981191146498,
-1.60868086595148));
#33919=CARTESIAN_POINT('Ctrl Pts',(-14.7602611194415,0.867979302403128,
-1.62010913746279));
#33920=CARTESIAN_POINT('Ctrl Pts',(-14.6492215994288,1.83175592377073,-0.151036162628272));
#33921=CARTESIAN_POINT('Ctrl Pts',(-14.5381820794161,1.12162251930453,1.4560579009365));
#33922=CARTESIAN_POINT('Ctrl Pts',(-14.4271425594034,-0.613481054986446,
1.73256534706872));
#33923=CARTESIAN_POINT('Ctrl Pts',(-14.3161030393907,-1.78796840564486,
0.425805903090126));
#33924=CARTESIAN_POINT('Ctrl Pts',(-14.205063519378,-1.32855999473149,-1.27006693803504));
#33925=CARTESIAN_POINT('Ctrl Pts',(-14.0940239993653,0.344923864904767,
-1.8053169289933));
#33926=CARTESIAN_POINT('Ctrl Pts',(-13.9829844793526,1.70320660624744,-0.690817590341849));
#33927=CARTESIAN_POINT('Ctrl Pts',(-13.8719449593399,1.50505129966774,1.05497027069917));
#33928=CARTESIAN_POINT('Ctrl Pts',(-13.7609054393273,-0.0684621685615409,
1.83669665926807));
#33929=CARTESIAN_POINT('Ctrl Pts',(-13.6498659193145,-1.57941298373299,
0.939998039097045));
#33930=CARTESIAN_POINT('Ctrl Pts',(-13.5388263993019,-1.64705184118444,
-0.815697198194015));
#33931=CARTESIAN_POINT('Ctrl Pts',(-13.4277868792892,-0.209568452681189,
-1.82598541898106));
#33932=CARTESIAN_POINT('Ctrl Pts',(-13.3167473592765,1.4194244756517,-1.1676368633319));
#33933=CARTESIAN_POINT('Ctrl Pts',(-13.2057078392638,1.75130743978355,0.557731062474938));
#33934=CARTESIAN_POINT('Ctrl Pts',(-13.0946683192511,0.482796462927691,
1.77342867408733));
#33935=CARTESIAN_POINT('Ctrl Pts',(-12.9836287992384,-1.22690748578881,
1.36851733931507));
#33936=CARTESIAN_POINT('Ctrl Pts',(-12.8725892792257,-1.81542890435427,
-0.286983588251427));
#33937=CARTESIAN_POINT('Ctrl Pts',(-12.761549759213,-0.744960386131938,
-1.68023085014673));
#33938=CARTESIAN_POINT('Ctrl Pts',(-12.6505102392003,1.00627386240032,-1.53803595554219));
#33939=CARTESIAN_POINT('Ctrl Pts',(-12.5394707191877,1.83794678447648,0.00965940594506788));
#33940=CARTESIAN_POINT('Ctrl Pts',(-12.4284311991749,0.990052298275348,
1.5485277309013));
#33941=CARTESIAN_POINT('Ctrl Pts',(-12.3173916791622,-0.762579793343959,
1.67230790988804));
#33942=CARTESIAN_POINT('Ctrl Pts',(-12.2063521591496,-1.8183450453305,0.267886137776231));
#33943=CARTESIAN_POINT('Ctrl Pts',(-12.0953126391368,-1.21245550897696,
-1.3813375132248));
#33944=CARTESIAN_POINT('Ctrl Pts',(-11.9842731191242,0.501409935092548,
-1.76825613633351));
#33945=CARTESIAN_POINT('Ctrl Pts',(-11.8732335991115,1.75707289349663,-0.539292623378071));
#33946=CARTESIAN_POINT('Ctrl Pts',(-11.7621940790988,1.40707327733112,1.18249164010207));
#33947=CARTESIAN_POINT('Ctrl Pts',(-11.6511545590861,-0.228749431006459,
1.82368182107101));
#33948=CARTESIAN_POINT('Ctrl Pts',(-11.5401150390734,-1.65553448263634,
0.798340318092896));
#33949=CARTESIAN_POINT('Ctrl Pts',(-11.4290755190607,-1.56944561223521,
-0.956546996715934));
#33950=CARTESIAN_POINT('Ctrl Pts',(-11.318035999048,-0.0491532482193918,
-1.83731479199404));
#33951=CARTESIAN_POINT('Ctrl Pts',(-11.2069964790353,1.51605673496666,-1.03909271148097));
#33952=CARTESIAN_POINT('Ctrl Pts',(-11.0959569590226,1.69585148053222,0.708681481814863));
#33953=CARTESIAN_POINT('Ctrl Pts',(-10.9849174390099,0.325929498694267,
1.80884262681183));
#33954=CARTESIAN_POINT('Ctrl Pts',(-10.8738779189972,-1.34183601595248,
1.25603256047899));
#33955=CARTESIAN_POINT('Ctrl Pts',(-10.7628383989846,-1.78339408069835,
-0.444575347517961));
#33956=CARTESIAN_POINT('Ctrl Pts',(-10.6517988789718,-0.595236530522984,
-1.73891781272768));
#33957=CARTESIAN_POINT('Ctrl Pts',(-10.5407593589592,1.1368648842552,-1.44418832623659));
#33958=CARTESIAN_POINT('Ctrl Pts',(-10.4297198389465,1.83006722788652,0.170281026853745));
#33959=CARTESIAN_POINT('Ctrl Pts',(-10.3186803189338,0.850902723426497,
1.62914279360528));
#33960=CARTESIAN_POINT('Ctrl Pts',(-10.2076407989211,-0.905840595584799,
1.59924810522983));
#33961=CARTESIAN_POINT('Ctrl Pts',(-10.0966012789084,-1.83480132900177,
0.107915567848148));
#33962=CARTESIAN_POINT('Ctrl Pts',(-9.98556175889571,-1.08706905972496,
-1.48203324729215));
#33963=CARTESIAN_POINT('Ctrl Pts',(-9.874522238883,0.654057457242615,-1.71765844372971));
#33964=CARTESIAN_POINT('Ctrl Pts',(-9.76348271887031,1.79748789421279,-0.38363909713309));
#33965=CARTESIAN_POINT('Ctrl Pts',(-9.65244319885762,1.29832339351032,1.30096043466144));
#33966=CARTESIAN_POINT('Ctrl Pts',(-9.54140367884492,-0.387285500229918,
1.79670577112734));
#33967=CARTESIAN_POINT('Ctrl Pts',(-9.43036415883223,-1.71898202317764,
0.65057089596963));
#33968=CARTESIAN_POINT('Ctrl Pts',(-9.31932463881954,-1.47982447900607,
-1.09007394154023));
#33969=CARTESIAN_POINT('Ctrl Pts',(-9.20828511880685,0.111638249353674,
-1.83457858593517));
#33970=CARTESIAN_POINT('Ctrl Pts',(-9.09724559879415,1.60108280900731,-0.902593776508504));
#33971=CARTESIAN_POINT('Ctrl Pts',(-8.98620607878146,1.62741291579734,0.854206584022058));
#33972=CARTESIAN_POINT('Ctrl Pts',(-8.87516655876877,0.166567378401736,
1.83040896936805));
#33973=CARTESIAN_POINT('Ctrl Pts',(-8.76412703875608,-1.44649210904326,
1.13393221365574));
#33974=CARTESIAN_POINT('Ctrl Pts',(-8.65308751874338,-1.73770646843612,
-0.598763656417053));
#33975=CARTESIAN_POINT('Ctrl Pts',(-8.5420479987307,-0.44095583657419,-1.78429247515137));
#33976=CARTESIAN_POINT('Ctrl Pts',(-8.43100847871798,1.25875262728536,-1.33928470087313));
#33977=CARTESIAN_POINT('Ctrl Pts',(-8.31996895870532,1.8081775760136,0.329599059907972));
#33978=CARTESIAN_POINT('Ctrl Pts',(-8.2089294386926,0.705239055515858,1.69728593974785));
#33979=CARTESIAN_POINT('Ctrl Pts',(-8.09788991867992,-1.04216672741466,
1.51394524305222));
#33980=CARTESIAN_POINT('Ctrl Pts',(-7.98685039866723,-1.83721127543857,
-0.0528811506306726));
#33981=CARTESIAN_POINT('Ctrl Pts',(-7.87581087865453,-0.953360544007956,
-1.57138326318549));
#33982=CARTESIAN_POINT('Ctrl Pts',(-7.76477135864184,0.80169783694629,-1.65391120224947));
#33983=CARTESIAN_POINT('Ctrl Pts',(-7.65373183862914,1.82414221101299,-0.225048618505586));
#33984=CARTESIAN_POINT('Ctrl Pts',(-7.54269231861645,1.17963418386913,1.40946971550936));
#33985=CARTESIAN_POINT('Ctrl Pts',(-7.43165279860376,-0.54285670200082,
1.75597502481768));
#33986=CARTESIAN_POINT('Ctrl Pts',(-7.32061327859107,-1.76926988216876,
0.49782102279954));
#33987=CARTESIAN_POINT('Ctrl Pts',(-7.20957375857836,-1.37887453684738,
-1.21525581600112));
#33988=CARTESIAN_POINT('Ctrl Pts',(-7.09853423856569,0.271575099355961,
-1.81779774785327));
#33989=CARTESIAN_POINT('Ctrl Pts',(-6.98749471855298,1.67385177993814,-0.75918502717621));
#33990=CARTESIAN_POINT('Ctrl Pts',(-6.8764551985403,1.54651567759537,0.993192300434498));
#33991=CARTESIAN_POINT('Ctrl Pts',(-6.7654156785276,0.00593010012215213,
1.83796260043647));
#33992=CARTESIAN_POINT('Ctrl Pts',(-6.65437615851491,-1.54007456944727,
1.00315103909255));
#33993=CARTESIAN_POINT('Ctrl Pts',(-6.54333663850221,-1.67871582947318,
-0.748368125033921));
#33994=CARTESIAN_POINT('Ctrl Pts',(-6.43229711848952,-0.283299401454877,
-1.81600747130234));
#33995=CARTESIAN_POINT('Ctrl Pts',(-6.32125759847683,1.37100397883372,-1.22412817005115));
#33996=CARTESIAN_POINT('Ctrl Pts',(-6.21021807846413,1.77244540527444,0.486393844545889));
#33997=CARTESIAN_POINT('Ctrl Pts',(-6.09917855845144,0.55417642399643,1.75243549889208));
#33998=CARTESIAN_POINT('Ctrl Pts',(-5.98813903843875,-1.17051454296774,
1.4170523601447));
#33999=CARTESIAN_POINT('Ctrl Pts',(-5.87709951842606,-1.82555643527539,
-0.213273037009483));
#34000=CARTESIAN_POINT('Ctrl Pts',(-5.76605999841336,-0.812353568509229,
-1.64870354109554));
#34001=CARTESIAN_POINT('Ctrl Pts',(-5.65502047840067,0.943200812016622,
-1.57750242944403));
#34002=CARTESIAN_POINT('Ctrl Pts',(-5.54398095838797,1.83683179154747,-0.0647352782582765));
#34003=CARTESIAN_POINT('Ctrl Pts',(-5.43294143837528,1.05191427466497,1.50718878892018));
#34004=CARTESIAN_POINT('Ctrl Pts',(-5.32190191836259,-0.694272059656186,
1.70180139671801));
#34005=CARTESIAN_POINT('Ctrl Pts',(-5.2108623983499,-1.80601308047596,0.341260076540456));
#34006=CARTESIAN_POINT('Ctrl Pts',(-5.0998228783372,-1.26736860890297,-1.33113428919024));
#34007=CARTESIAN_POINT('Ctrl Pts',(-4.98878335832452,0.429432903867215,
-1.78710074359752));
#34008=CARTESIAN_POINT('Ctrl Pts',(-4.87774383831181,1.73380656428109,-0.6099643303886));
#34009=CARTESIAN_POINT('Ctrl Pts',(-4.76670431829913,1.45377907542383,1.12457462471391));
#34010=CARTESIAN_POINT('Ctrl Pts',(-4.65566479828643,-0.154752576089497,
1.83144569312997));
#34011=CARTESIAN_POINT('Ctrl Pts',(-4.54462527827374,-1.62186697584008,
0.864690233187587));
#34012=CARTESIAN_POINT('Ctrl Pts',(-4.43358575826105,-1.60687376714965,
-0.892243455082156));
#34013=CARTESIAN_POINT('Ctrl Pts',(-4.32254623824836,-0.123474165349735,
-1.83382000675687));
#34014=CARTESIAN_POINT('Ctrl Pts',(-4.21150671823566,1.4727595977204,-1.09960031557524));
#34015=CARTESIAN_POINT('Ctrl Pts',(-4.10046719822297,1.72314426360711,0.639465036955492));
#34016=CARTESIAN_POINT('Ctrl Pts',(-3.98942767821027,0.398871290133161,
1.79416927311721));
#34017=CARTESIAN_POINT('Ctrl Pts',(-3.87838815819758,-1.28990147444681,
1.30931122079946));
#34018=CARTESIAN_POINT('Ctrl Pts',(-3.76734863818489,-1.79992603224029,
-0.372032209833472));
#34019=CARTESIAN_POINT('Ctrl Pts',(-3.6563091181722,-0.665127613333747,
-1.71340215497423));
#34020=CARTESIAN_POINT('Ctrl Pts',(-3.5452695981595,1.07748310522118,-1.48901707332687));
#34021=CARTESIAN_POINT('Ctrl Pts',(-3.43423007814681,1.83545949062223,0.0960736434662692));
#34022=CARTESIAN_POINT('Ctrl Pts',(-3.32319055813411,0.916141426756487,
1.59336956568948));
#34023=CARTESIAN_POINT('Ctrl Pts',(-3.21215103812143,-0.840372411640004,
1.63459961350804));
#34024=CARTESIAN_POINT('Ctrl Pts',(-3.10111151810872,-1.82893033021795,
0.18208661083865));
#34025=CARTESIAN_POINT('Ctrl Pts',(-2.99007199809604,-1.14616032978072,
-1.43682225244029));
#34026=CARTESIAN_POINT('Ctrl Pts',(-2.87903247808334,0.584003181164767,
-1.74272257439688));
#34027=CARTESIAN_POINT('Ctrl Pts',(-2.76799295807065,1.78048817758317,-0.456074046366774));
#34028=CARTESIAN_POINT('Ctrl Pts',(-2.65695343805795,1.34991305530291,1.24734775817125));
#34029=CARTESIAN_POINT('Ctrl Pts',(-2.54591391804527,-0.314250542958959,
1.81090813803855));
#34030=CARTESIAN_POINT('Ctrl Pts',(-2.43487439803257,-1.69124316513835,
0.719609783155264));
#34031=CARTESIAN_POINT('Ctrl Pts',(-2.32383487801988,-1.52273027016296,
-1.02928820647559));
#34032=CARTESIAN_POINT('Ctrl Pts',(-2.21279535800718,0.0372963305200237,
-1.8375937199123));
#34033=CARTESIAN_POINT('Ctrl Pts',(-2.10175583799449,1.56324048867835,-0.966654456903947));
#34034=CARTESIAN_POINT('Ctrl Pts',(-1.9907163179818,1.66065158442465,0.787640790575088));
#34035=CARTESIAN_POINT('Ctrl Pts',(-1.87967679796911,0.2405125782874,1.82216778579164));
#34036=CARTESIAN_POINT('Ctrl Pts',(-1.76863727795641,-1.39941352484514,
1.19154660657962));
#34037=CARTESIAN_POINT('Ctrl Pts',(-1.65759775794372,-1.760516335917,-0.527943226680482));
#34038=CARTESIAN_POINT('Ctrl Pts',(-1.54655823793103,-0.512809661837298,
-1.76498391861309));
#34039=CARTESIAN_POINT('Ctrl Pts',(-1.43551871791833,1.20351651524581,-1.3891323162764));
#34040=CARTESIAN_POINT('Ctrl Pts',(-1.32447919790564,1.82003619839053,0.256146657758448));
#34041=CARTESIAN_POINT('Ctrl Pts',(-1.21343967789295,0.77335431875082,1.66735307747278));
#34042=CARTESIAN_POINT('Ctrl Pts',(-1.10240015788025,-0.980037893435529,
1.55488263712548));
#34043=CARTESIAN_POINT('Ctrl Pts',(-0.991360637867559,-1.837848836859,0.0215220372239174));
#34044=CARTESIAN_POINT('Ctrl Pts',(-0.88032111785487,-1.01617257076799,
-1.53151604812273));
#34045=CARTESIAN_POINT('Ctrl Pts',(-0.769281597842172,0.734093027864279,
-1.68499263158297));
#34046=CARTESIAN_POINT('Ctrl Pts',(-0.658242077829484,1.81355749436498,
-0.29871196954151));
#34047=CARTESIAN_POINT('Ctrl Pts',(-0.547202557816791,1.23567804673567,
1.36060926789406));
#34048=CARTESIAN_POINT('Ctrl Pts',(-0.436163037804095,-0.47127670149265,
1.77643588465474));
#34049=CARTESIAN_POINT('Ctrl Pts',(-0.3251235177914,-1.74779774243877,0.569156001613867));
#34050=CARTESIAN_POINT('Ctrl Pts',(-0.214083997778712,-1.42669014007662,
-1.15871157842014));
#34051=CARTESIAN_POINT('Ctrl Pts',(-0.103044477766015,0.197324521003166,
-1.82680605937946));
#34052=CARTESIAN_POINT('Ctrl Pts',(0.00799504224667571,1.64263470516183,
-0.827265704348207));
#34053=CARTESIAN_POINT('Ctrl Pts',(0.119034562259368,1.58367018209927,0.931762477007397));
#34054=CARTESIAN_POINT('Ctrl Pts',(0.1930609089345,0.584258987358921,1.53143275677265));
#34055=CARTESIAN_POINT('Ctrl Pts',(0.230074082272065,0.0679696520801858,
1.55401427805413));
#34056=CARTESIAN_POINT('',(0.,0.0853826423430472,1.95213365433479));
#34057=CARTESIAN_POINT('Ctrl Pts',(2.77555756156289E-17,1.33819577673882,
-0.797970124357286));
#34058=CARTESIAN_POINT('Ctrl Pts',(1.85767714458696E-16,1.36144302530136,
-0.768447784071024));
#34059=CARTESIAN_POINT('Ctrl Pts',(4.34722244779448E-15,1.38350431609264,
-0.738083050538838));
#34060=CARTESIAN_POINT('Ctrl Pts',(3.30291349825984E-15,1.40431382449103,
-0.706922234106086));
#34061=CARTESIAN_POINT('Ctrl Pts',(1.64949265289499E-15,1.43726085131009,
-0.657586313475071));
#34062=CARTESIAN_POINT('Ctrl Pts',(-1.84250246973165E-15,1.46707229630311,
-0.606256863967469));
#34063=CARTESIAN_POINT('Ctrl Pts',(-1.2490009027033E-15,1.49380501049835,
-0.553258599699532));
#34064=CARTESIAN_POINT('Ctrl Pts',(-9.0035866934265E-16,1.50950868121903,
-0.522125685744261));
#34065=CARTESIAN_POINT('Ctrl Pts',(-6.10224942617705E-15,1.52414930935612,
-0.49041610674948));
#34066=CARTESIAN_POINT('Ctrl Pts',(-5.71764857681956E-15,1.53773259716531,
-0.458190051451294));
#34067=CARTESIAN_POINT('Ctrl Pts',(-5.5403078360827E-15,1.54399589670235,
-0.443330509338595));
#34068=CARTESIAN_POINT('Ctrl Pts',(1.3347825398265E-15,1.55003513608504,
-0.428358552453907));
#34069=CARTESIAN_POINT('Ctrl Pts',(1.11022302462516E-15,1.55584236110343,
-0.413302430982821));
#34070=CARTESIAN_POINT('Ctrl Pts',(2.43036775803427E-16,1.57826824528491,
-0.355159886951195));
#34071=CARTESIAN_POINT('Ctrl Pts',(3.22432105167343E-16,1.59726695275495,
-0.295698115059786));
#34072=CARTESIAN_POINT('Ctrl Pts',(1.66533453693773E-16,1.61289818059431,
-0.235272160005541));
#34073=CARTESIAN_POINT('Ctrl Pts',(4.64879345376463E-17,1.62493458272665,
-0.188742795726714));
#34074=CARTESIAN_POINT('Ctrl Pts',(4.60117079108609E-15,1.63497355098178,
-0.141640714047145));
#34075=CARTESIAN_POINT('Ctrl Pts',(6.02295990859147E-15,1.64302567919564,
-0.0941152689092269));
#34076=CARTESIAN_POINT('Ctrl Pts',(6.50794676775413E-15,1.64577234276476,
-0.0779038518404372));
#34077=CARTESIAN_POINT('Ctrl Pts',(-2.48752701466179E-15,1.6482876960855,
-0.0616430990017152));
#34078=CARTESIAN_POINT('Ctrl Pts',(-2.22044604925031E-15,1.65057175197968,
-0.0453387342717473));
#34079=CARTESIAN_POINT('Ctrl Pts',(-1.95995858369583E-15,1.65279942076971,
-0.0294368797931177));
#34080=CARTESIAN_POINT('Ctrl Pts',(2.01657362464638E-16,1.65480738528587,
-0.0134894297485523));
#34081=CARTESIAN_POINT('Ctrl Pts',(1.66533453693773E-16,1.65659278118466,
0.00247052324260472));
#34082=CARTESIAN_POINT('Ctrl Pts',(2.50013631112385E-17,1.66378704921789,
0.0667812902239603));
#34083=CARTESIAN_POINT('Ctrl Pts',(2.78729284858849E-15,1.66738409972544,
0.131373953612928));
#34084=CARTESIAN_POINT('Ctrl Pts',(2.22044604925031E-15,1.66744264184217,
0.19588728583938));
#34085=CARTESIAN_POINT('Ctrl Pts',(1.64177178678514E-15,1.6675024054613,
0.261746712035136));
#34086=CARTESIAN_POINT('Ctrl Pts',(2.74120336787342E-15,1.6638748341243,
0.327524480561884));
#34087=CARTESIAN_POINT('Ctrl Pts',(1.85962356624714E-15,1.65657462015792,
0.392860803376907));
#34088=CARTESIAN_POINT('Ctrl Pts',(1.27711720799663E-15,1.65175098304174,
0.43603196427947));
#34089=CARTESIAN_POINT('Ctrl Pts',(-9.10818389979693E-16,1.64532289717713,
0.479010876745845));
#34090=CARTESIAN_POINT('Ctrl Pts',(-5.55111512312578E-16,1.63728231888051,
0.521695995682809));
#34091=CARTESIAN_POINT('Ctrl Pts',(-3.80822141106348E-16,1.63334259372073,
0.542610864094066));
#34092=CARTESIAN_POINT('Ctrl Pts',(-3.4150718129913E-15,1.62901558792228,
0.56345520655164));
#34093=CARTESIAN_POINT('Ctrl Pts',(-3.71924713249427E-15,1.62429946022137,
0.584217038477149));
#34094=CARTESIAN_POINT('Ctrl Pts',(-3.90626465249348E-15,1.62139982159171,
0.596982131725653));
#34095=CARTESIAN_POINT('Ctrl Pts',(3.41061712681253E-15,1.61835307480705,
0.609716033053302));
#34096=CARTESIAN_POINT('Ctrl Pts',(3.71924713249427E-15,1.61515867855561,
0.622415937599459));
#34097=CARTESIAN_POINT('Ctrl Pts',(3.9772647208833E-15,1.61248813323602,
0.633033177282724));
#34098=CARTESIAN_POINT('Ctrl Pts',(-2.16347027594684E-15,1.60971491624366,
0.643624280439148));
#34099=CARTESIAN_POINT('Ctrl Pts',(-2.16493489801906E-15,1.60684190188332,
0.654177060515785));
#34100=CARTESIAN_POINT('Ctrl Pts',(-2.17400880471352E-15,1.58904245400387,
0.719555661315922));
#34101=CARTESIAN_POINT('Ctrl Pts',(-2.56174063694999E-15,1.56738808989198,
0.783577323980778));
#34102=CARTESIAN_POINT('Ctrl Pts',(-2.23432383705813E-15,1.5419084220951,
0.845867575772783));
#34103=CARTESIAN_POINT('Ctrl Pts',(-2.15110675602605E-15,1.53543244535713,
0.861699423535622));
#34104=CARTESIAN_POINT('Ctrl Pts',(1.01114729712598E-15,1.52870910174203,
0.87741947571057));
#34105=CARTESIAN_POINT('Ctrl Pts',(9.43689570931383E-16,1.52173834456087,
0.893021649046084));
#34106=CARTESIAN_POINT('Ctrl Pts',(7.03007412007331E-16,1.49528259824579,
0.952235752908995));
#34107=CARTESIAN_POINT('Ctrl Pts',(-1.51979766192264E-15,1.46526720058678,
1.00975289709403));
#34108=CARTESIAN_POINT('Ctrl Pts',(-3.33066907387547E-16,1.43198511538068,
1.06544449418259));
#34109=CARTESIAN_POINT('Ctrl Pts',(3.10283512530559E-16,1.41394223293977,
1.09563602013396));
#34110=CARTESIAN_POINT('Ctrl Pts',(5.3238620172534E-15,1.39493838269964,
1.12529083901457));
#34111=CARTESIAN_POINT('Ctrl Pts',(5.59274848654923E-15,1.37501431840528,
1.1543865469354));
#34112=CARTESIAN_POINT('Ctrl Pts',(5.79604585589064E-15,1.35995030321613,
1.17638497956356));
#34113=CARTESIAN_POINT('Ctrl Pts',(3.98761921311371E-15,1.34436016743568,
1.19806377318932));
#34114=CARTESIAN_POINT('Ctrl Pts',(4.63518112781003E-15,1.32826011938545,
1.21941254397355));
#34115=CARTESIAN_POINT('Ctrl Pts',(5.00670657023675E-15,1.31902304515486,
1.23166096583232));
#34116=CARTESIAN_POINT('Ctrl Pts',(-2.81519590396613E-15,1.30961522599116,
1.24380414149294));
#34117=CARTESIAN_POINT('Ctrl Pts',(-2.76167977375508E-15,1.30005809876754,
1.25581735673097));
#34118=CARTESIAN_POINT('Ctrl Pts',(-2.52523500380136E-15,1.2578328343679,
1.3088941001756));
#34119=CARTESIAN_POINT('Ctrl Pts',(-4.17224765824516E-15,1.21263786762318,
1.35951742488655));
#34120=CARTESIAN_POINT('Ctrl Pts',(-2.99760216648792E-15,1.16481156614242,
1.40755648980915));
#34121=CARTESIAN_POINT('Ctrl Pts',(-1.7982525475441E-15,1.1159794232883,
1.45660587076164));
#34122=CARTESIAN_POINT('Ctrl Pts',(-2.21069601816558E-18,1.06440359303693,
1.50296188609699));
#34123=CARTESIAN_POINT('Ctrl Pts',(-6.73072708679001E-16,1.01039246439479,
1.54646595937401));
#34124=CARTESIAN_POINT('Ctrl Pts',(-1.3489991402192E-15,0.955973599177281,
1.59029845018829));
#34125=CARTESIAN_POINT('Ctrl Pts',(-1.1547791066913E-16,0.899081837248503,
1.63123654739737));
#34126=CARTESIAN_POINT('Ctrl Pts',(1.33226762955019E-15,0.839989874352363,
1.66908726954678));
#34127=CARTESIAN_POINT('Ctrl Pts',(1.69882738300955E-15,0.825028173729644,
1.67867082618288));
#34128=CARTESIAN_POINT('Ctrl Pts',(-5.43398623855677E-16,0.809925242478508,
1.68805627460793));
#34129=CARTESIAN_POINT('Ctrl Pts',(-7.21644966006352E-16,0.79468516045783,
1.69724007942585));
#34130=CARTESIAN_POINT('Ctrl Pts',(-8.49633924018289E-16,0.783742090354353,
1.70383446781581));
#34131=CARTESIAN_POINT('Ctrl Pts',(7.66742462836056E-16,0.772727015708312,
1.71032552223986));
#34132=CARTESIAN_POINT('Ctrl Pts',(6.93889390390723E-16,0.761657574914039,
1.71670288403641));
#34133=CARTESIAN_POINT('Ctrl Pts',(2.82215011875755E-16,0.69910695067084,
1.7527397506508));
#34134=CARTESIAN_POINT('Ctrl Pts',(-3.781339996231E-15,0.634711960700427,
1.78521757183589));
#34135=CARTESIAN_POINT('Ctrl Pts',(-4.03843625207401E-15,0.568806275526336,
1.81397636836835));
#34136=CARTESIAN_POINT('Ctrl Pts',(-4.29614369899938E-15,0.502743913752955,
1.84280353275751));
#34137=CARTESIAN_POINT('Ctrl Pts',(-1.97887160151066E-15,0.435162865154654,
1.86789472013933));
#34138=CARTESIAN_POINT('Ctrl Pts',(-2.9767854847762E-15,0.366360222072395,
1.88905407399748));
#34139=CARTESIAN_POINT('Ctrl Pts',(-3.9534463475613E-15,0.299022899802941,
1.90976278758652));
#34140=CARTESIAN_POINT('Ctrl Pts',(2.03258476747404E-15,0.230514597231587,
1.92670591644718));
#34141=CARTESIAN_POINT('Ctrl Pts',(2.71224015468974E-15,0.161089063758093,
1.93965721286968));
#34142=CARTESIAN_POINT('Ctrl Pts',(2.95814837249331E-15,0.13596999676082,
1.94434316148629));
#34143=CARTESIAN_POINT('Ctrl Pts',(3.98524470648727E-17,0.110730680189629,
1.94850609293125));
#34144=CARTESIAN_POINT('Ctrl Pts',(-1.38777878078145E-17,0.0853826423430475,
1.95213365433479));
#34145=CARTESIAN_POINT('Ctrl Pts',(-1.73472347597681E-17,0.0853826423430476,
1.95213365433479));
#34146=CARTESIAN_POINT('Ctrl Pts',(-0.0370131733375648,0.733938965798307,
1.92376702457974));
#34147=CARTESIAN_POINT('Ctrl Pts',(-0.0740263466751305,1.36166300132472,
1.54711780353787));
#34148=CARTESIAN_POINT('Ctrl Pts',(-0.111039520012696,1.68787010406214,
0.990514925967878));
#34149=CARTESIAN_POINT('Ctrl Pts',(-0.148052693350262,2.01407720679956,
0.433912048397882));
#34150=CARTESIAN_POINT('Ctrl Pts',(-0.185065866687825,2.03876737674798,
-0.302644485700221));
#34151=CARTESIAN_POINT('Ctrl Pts',(-0.222079040025389,1.7485156439952,-0.880191139520007));
#34152=CARTESIAN_POINT('Ctrl Pts',(-0.259092213362953,1.45826391124243,
-1.45773779333978));
#34153=CARTESIAN_POINT('Ctrl Pts',(-0.296105386700518,0.853070275788427,
-1.87627456688123));
#34154=CARTESIAN_POINT('Ctrl Pts',(-0.333118560038082,0.210462245402071,
-1.94566760641157));
#34155=CARTESIAN_POINT('Ctrl Pts',(-0.370131733375646,-0.432145784984285,
-2.01506064594191));
#34156=CARTESIAN_POINT('Ctrl Pts',(-0.407144906713211,-1.11216821030301,
-1.73530995146117));
#34157=CARTESIAN_POINT('Ctrl Pts',(-0.444158080050774,-1.51940799416304,
-1.23368026463156));
#34158=CARTESIAN_POINT('Ctrl Pts',(-0.469482155992443,-1.79803774360075,
-0.890469803642078));
#34159=CARTESIAN_POINT('Ctrl Pts',(-0.494806231934111,-1.94897325447817,
-0.443393976333821));
#34160=CARTESIAN_POINT('Ctrl Pts',(-0.520130307875779,-1.95245178959834,
0.00157515171675247));
#34161=CARTESIAN_POINT('Origin',(0.329462113107775,0.,0.));
#34162=CARTESIAN_POINT('',(-0.0510757737844506,0.,0.));
#34163=CARTESIAN_POINT('',(0.7,-1.23357587978679,1.51069475268627E-16));
#34164=CARTESIAN_POINT('',(0.329462113107775,-0.625,-7.65404249467096E-17));
#34165=CARTESIAN_POINT('Origin',(0.7,0.,0.));
#34166=CARTESIAN_POINT('Origin',(2.3,-2.77555756156289E-16,-1.44337567297406));
#34167=CARTESIAN_POINT('',(2.08323056361362,-2.65143809681227E-16,-1.44337567297406));
#34168=CARTESIAN_POINT('',(2.08323056361362,-1.25,-0.721687836487032));
#34169=CARTESIAN_POINT('Ctrl Pts',(2.08323056361362,-5.89805981832114E-16,
-1.44337567297406));
#34170=CARTESIAN_POINT('Ctrl Pts',(2.11697695076186,-0.213078403143805,
-1.32035479956049));
#34171=CARTESIAN_POINT('Ctrl Pts',(2.13099428157845,-0.425048382906795,
-1.19797387468421));
#34172=CARTESIAN_POINT('Ctrl Pts',(2.13099428157845,-0.824951617093206,
-0.967089634776885));
#34173=CARTESIAN_POINT('Ctrl Pts',(2.11697695076186,-1.0369215968562,-0.844708709900604));
#34174=CARTESIAN_POINT('Ctrl Pts',(2.08323056361362,-1.25,-0.721687836487033));
#34175=CARTESIAN_POINT('',(0.7,-2.77555756156289E-16,-1.44337567297406));
#34176=CARTESIAN_POINT('',(2.3,-2.65143809681227E-16,-1.44337567297406));
#34177=CARTESIAN_POINT('',(0.7,-1.25,-0.721687836487032));
#34178=CARTESIAN_POINT('',(0.7,-1.25,-0.721687836487032));
#34179=CARTESIAN_POINT('',(2.3,-1.25,-0.721687836487032));
#34180=CARTESIAN_POINT('Origin',(2.3,-1.25,-0.721687836487032));
#34181=CARTESIAN_POINT('',(2.08323056361362,-1.25,0.721687836487032));
#34182=CARTESIAN_POINT('Ctrl Pts',(2.08323056361362,-1.25,-0.721687836487033));
#34183=CARTESIAN_POINT('Ctrl Pts',(2.11697695076186,-1.25,-0.475646089659891));
#34184=CARTESIAN_POINT('Ctrl Pts',(2.13099428157846,-1.25,-0.230884239907327));
#34185=CARTESIAN_POINT('Ctrl Pts',(2.13099428157846,-1.25,0.230884239907327));
#34186=CARTESIAN_POINT('Ctrl Pts',(2.11697695076186,-1.25,0.475646089659889));
#34187=CARTESIAN_POINT('Ctrl Pts',(2.08323056361362,-1.25,0.721687836487032));
#34188=CARTESIAN_POINT('',(0.7,-1.25,0.721687836487032));
#34189=CARTESIAN_POINT('',(0.7,-1.25,0.721687836487032));
#34190=CARTESIAN_POINT('',(2.3,-1.25,0.721687836487032));
#34191=CARTESIAN_POINT('Origin',(2.3,-1.25,0.721687836487032));
#34192=CARTESIAN_POINT('',(2.08323056361362,8.83812698937422E-17,1.44337567297406));
#34193=CARTESIAN_POINT('Ctrl Pts',(2.08323056361362,-1.25,0.721687836487032));
#34194=CARTESIAN_POINT('Ctrl Pts',(2.11697695076186,-1.0369215968562,0.844708709900604));
#34195=CARTESIAN_POINT('Ctrl Pts',(2.13099428157845,-0.824951617093207,
0.967089634776885));
#34196=CARTESIAN_POINT('Ctrl Pts',(2.13099428157846,-0.425048382906794,
1.19797387468421));
#34197=CARTESIAN_POINT('Ctrl Pts',(2.11697695076186,-0.213078403143805,
1.32035479956049));
#34198=CARTESIAN_POINT('Ctrl Pts',(2.08323056361362,3.46944695195361E-17,
1.44337567297406));
#34199=CARTESIAN_POINT('',(0.7,1.38777878078145E-16,1.44337567297406));
#34200=CARTESIAN_POINT('',(0.7,8.83812698937422E-17,1.44337567297406));
#34201=CARTESIAN_POINT('',(2.3,8.83812698937422E-17,1.44337567297406));
#34202=CARTESIAN_POINT('Origin',(2.3,0.,1.44337567297406));
#34203=CARTESIAN_POINT('',(2.08323056361362,1.25,0.721687836487032));
#34204=CARTESIAN_POINT('Ctrl Pts',(2.08323056361362,0.,1.44337567297406));
#34205=CARTESIAN_POINT('Ctrl Pts',(2.11697695076186,0.213078403143805,1.32035479956049));
#34206=CARTESIAN_POINT('Ctrl Pts',(2.13099428157846,0.425048382906794,1.19797387468421));
#34207=CARTESIAN_POINT('Ctrl Pts',(2.13099428157846,0.824951617093207,0.967089634776885));
#34208=CARTESIAN_POINT('Ctrl Pts',(2.11697695076186,1.0369215968562,0.844708709900604));
#34209=CARTESIAN_POINT('Ctrl Pts',(2.08323056361362,1.25,0.721687836487032));
#34210=CARTESIAN_POINT('',(0.7,1.25,0.721687836487032));
#34211=CARTESIAN_POINT('',(0.7,1.25,0.721687836487032));
#34212=CARTESIAN_POINT('',(2.3,1.25,0.721687836487032));
#34213=CARTESIAN_POINT('Origin',(2.3,1.25,-0.721687836487033));
#34214=CARTESIAN_POINT('',(2.08323056361362,1.25,-0.721687836487033));
#34215=CARTESIAN_POINT('Ctrl Pts',(2.08323056361362,1.25,-0.721687836487033));
#34216=CARTESIAN_POINT('Ctrl Pts',(2.11697695076186,1.03692159685619,-0.844708709900604));
#34217=CARTESIAN_POINT('Ctrl Pts',(2.13099428157846,0.824951617093206,-0.967089634776885));
#34218=CARTESIAN_POINT('Ctrl Pts',(2.13099428157846,0.425048382906794,-1.19797387468421));
#34219=CARTESIAN_POINT('Ctrl Pts',(2.11697695076186,0.213078403143804,-1.32035479956049));
#34220=CARTESIAN_POINT('Ctrl Pts',(2.08323056361362,-8.67361737988404E-16,
-1.44337567297407));
#34221=CARTESIAN_POINT('',(0.7,1.25,-0.721687836487033));
#34222=CARTESIAN_POINT('',(2.3,1.25,-0.721687836487033));
#34223=CARTESIAN_POINT('',(0.7,-2.65143809681227E-16,-1.44337567297406));
#34224=CARTESIAN_POINT('Origin',(2.3,1.25,0.721687836487032));
#34225=CARTESIAN_POINT('Ctrl Pts',(2.08323056361362,1.25,0.721687836487032));
#34226=CARTESIAN_POINT('Ctrl Pts',(2.11697695076186,1.25,0.47564608965989));
#34227=CARTESIAN_POINT('Ctrl Pts',(2.13099428157846,1.25,0.230884239907327));
#34228=CARTESIAN_POINT('Ctrl Pts',(2.13099428157846,1.25,-0.230884239907328));
#34229=CARTESIAN_POINT('Ctrl Pts',(2.11697695076186,1.25,-0.47564608965989));
#34230=CARTESIAN_POINT('Ctrl Pts',(2.08323056361362,1.25,-0.721687836487033));
#34231=CARTESIAN_POINT('',(0.7,1.25,-0.721687836487033));
#34232=CARTESIAN_POINT('Origin',(0.7,0.,0.));
#34233=CARTESIAN_POINT('Origin',(-20.,1.6,0.));
#34234=CARTESIAN_POINT('',(-20.,-1.6,-1.95943487863576E-16));
#34235=CARTESIAN_POINT('Origin',(-20.,0.,0.));
#34236=CARTESIAN_POINT('Origin',(-19.8,0.,0.));
#34237=CARTESIAN_POINT('',(-19.8,-1.8,-2.20436423846524E-16));
#34238=CARTESIAN_POINT('Origin',(-9.8,0.,0.));
#34239=CARTESIAN_POINT('Origin',(0.,0.,0.));
#34240=CARTESIAN_POINT('Origin',(0.,3.8,0.));
#34241=CARTESIAN_POINT('',(1.73472347597681E-17,-3.8,-4.65365783675994E-16));
#34242=CARTESIAN_POINT('Origin',(0.,0.,0.));
#34243=CARTESIAN_POINT('Origin',(0.125,0.,0.));
#34244=CARTESIAN_POINT('',(0.25,-3.8,-4.65365783675994E-16));
#34245=CARTESIAN_POINT('',(0.25,-4.65365783675994E-16,3.8));
#34246=CARTESIAN_POINT('Origin',(0.25,0.,0.));
#34247=CARTESIAN_POINT('',(0.125,-3.8,-4.65365783675994E-16));
#34248=CARTESIAN_POINT('Origin',(0.25,0.,0.));
#34249=CARTESIAN_POINT('Ctrl Pts',(0.25,0.,3.8));
#34250=CARTESIAN_POINT('Ctrl Pts',(0.25,-3.8,3.8));
#34251=CARTESIAN_POINT('Ctrl Pts',(0.25,-3.8,0.));
#34252=CARTESIAN_POINT('Ctrl Pts',(0.25,-3.8,-3.8));
#34253=CARTESIAN_POINT('Ctrl Pts',(0.25,0.,-3.8));
#34254=CARTESIAN_POINT('Ctrl Pts',(0.25,3.8,-3.8));
#34255=CARTESIAN_POINT('Ctrl Pts',(0.25,3.8,0.));
#34256=CARTESIAN_POINT('Ctrl Pts',(0.25,3.8,3.8));
#34257=CARTESIAN_POINT('Ctrl Pts',(0.25,0.,3.8));
#34258=CARTESIAN_POINT('Ctrl Pts',(1.75830245810501,0.,2.94383864898856));
#34259=CARTESIAN_POINT('Ctrl Pts',(1.75830245810501,-2.94383864898856,2.94383864898856));
#34260=CARTESIAN_POINT('Ctrl Pts',(1.75830245810501,-2.94383864898856,0.));
#34261=CARTESIAN_POINT('Ctrl Pts',(1.75830245810501,-2.94383864898856,-2.94383864898856));
#34262=CARTESIAN_POINT('Ctrl Pts',(1.75830245810501,0.,-2.94383864898856));
#34263=CARTESIAN_POINT('Ctrl Pts',(1.75830245810501,2.94383864898856,-2.94383864898856));
#34264=CARTESIAN_POINT('Ctrl Pts',(1.75830245810501,2.94383864898856,0.));
#34265=CARTESIAN_POINT('Ctrl Pts',(1.75830245810501,2.94383864898856,2.94383864898856));
#34266=CARTESIAN_POINT('Ctrl Pts',(1.75830245810501,0.,2.94383864898856));
#34267=CARTESIAN_POINT('Ctrl Pts',(2.13099428157846,0.,1.25));
#34268=CARTESIAN_POINT('Ctrl Pts',(2.13099428157846,-1.25,1.25));
#34269=CARTESIAN_POINT('Ctrl Pts',(2.13099428157846,-1.25,0.));
#34270=CARTESIAN_POINT('Ctrl Pts',(2.13099428157846,-1.25,-1.25));
#34271=CARTESIAN_POINT('Ctrl Pts',(2.13099428157846,0.,-1.25));
#34272=CARTESIAN_POINT('Ctrl Pts',(2.13099428157846,1.25,-1.25));
#34273=CARTESIAN_POINT('Ctrl Pts',(2.13099428157846,1.25,0.));
#34274=CARTESIAN_POINT('Ctrl Pts',(2.13099428157846,1.25,1.25));
#34275=CARTESIAN_POINT('Ctrl Pts',(2.13099428157846,0.,1.25));
#34276=CARTESIAN_POINT('Ctrl Pts',(2.08323056361362,0.,1.44337567297407));
#34277=CARTESIAN_POINT('Ctrl Pts',(1.65564775032955,0.,3.00210878759666));
#34278=CARTESIAN_POINT('Ctrl Pts',(0.25,0.,3.8));
#34279=CARTESIAN_POINT('',(0.,0.,0.));
#34280=CARTESIAN_POINT('Origin',(0.7,0.,0.));
#34281=CARTESIAN_POINT('',(0.8,4.3,-5.26598123633362E-16));
#34282=CARTESIAN_POINT('Origin',(0.8,0.,0.));
#34283=CARTESIAN_POINT('',(0.6,4.5,5.51091059616309E-16));
#34284=CARTESIAN_POINT('',(0.7,4.4,5.38844591624835E-16));
#34285=CARTESIAN_POINT('',(0.6,-4.5,-5.51091059616309E-16));
#34286=CARTESIAN_POINT('Origin',(0.6,0.,0.));
#34287=CARTESIAN_POINT('Origin',(0.6,0.,0.));
#34288=CARTESIAN_POINT('Origin',(0.475,0.,0.));
#34289=CARTESIAN_POINT('',(0.15,-4.5,-5.51091059616309E-16));
#34290=CARTESIAN_POINT('',(0.475,-4.5,-5.51091059616309E-16));
#34291=CARTESIAN_POINT('Origin',(0.15,0.,0.));
#34292=CARTESIAN_POINT('Origin',(0.8,2.2,0.));
#34293=CARTESIAN_POINT('',(0.8,-2.2,-2.69422295812418E-16));
#34294=CARTESIAN_POINT('Origin',(0.8,0.,0.));
#34295=CARTESIAN_POINT('Origin',(0.4,0.,0.));
#34296=CARTESIAN_POINT('',(0.,-2.2,-2.69422295812418E-16));
#34297=CARTESIAN_POINT('',(0.4,-2.2,-2.69422295812418E-16));
#34298=CARTESIAN_POINT('Origin',(0.,0.,0.));
#34299=CARTESIAN_POINT('Origin',(0.,4.35,0.));
#34300=CARTESIAN_POINT('',(-3.20923843055709E-16,-4.35,-5.32721357629099E-16));
#34301=CARTESIAN_POINT('Origin',(0.,0.,0.));
#34302=CARTESIAN_POINT('Origin',(0.0749999999999999,0.,0.));
#34303=CARTESIAN_POINT('',(0.0749999999999999,-4.425,-5.41906208622704E-16));
#34304=CARTESIAN_POINT('',(0.,0.,0.));
#34305=CARTESIAN_POINT('Origin',(0.,3.41339745962156,1.97072594216369));
#34306=CARTESIAN_POINT('',(2.84579300863683,3.32679491924311,2.12072594216369));
#34307=CARTESIAN_POINT('',(2.84579300863683,3.5,1.82072594216369));
#34308=CARTESIAN_POINT('Ctrl Pts',(2.84579300863683,3.32679491924311,2.12072594216369));
#34309=CARTESIAN_POINT('Ctrl Pts',(2.85025803029788,3.41339745962156,1.97072594216368));
#34310=CARTESIAN_POINT('Ctrl Pts',(2.84579300863683,3.5,1.82072594216369));
#34311=CARTESIAN_POINT('',(0.35420699136317,3.5,1.82072594216369));
#34312=CARTESIAN_POINT('',(0.,3.5,1.82072594216369));
#34313=CARTESIAN_POINT('',(0.35420699136317,3.32679491924311,2.12072594216369));
#34314=CARTESIAN_POINT('Ctrl Pts',(0.35420699136317,3.5,1.82072594216369));
#34315=CARTESIAN_POINT('Ctrl Pts',(0.349741969702116,3.41339745962155,1.9707259421637));
#34316=CARTESIAN_POINT('Ctrl Pts',(0.35420699136317,3.32679491924311,2.12072594216369));
#34317=CARTESIAN_POINT('',(0.,3.32679491924311,2.12072594216369));
#34318=CARTESIAN_POINT('Origin',(0.,3.5,-2.02072594216369));
#34319=CARTESIAN_POINT('',(2.84579300863683,3.5,-1.82072594216369));
#34320=CARTESIAN_POINT('Ctrl Pts',(2.84579300863683,3.5,1.82072594216369));
#34321=CARTESIAN_POINT('Ctrl Pts',(3.3391842955686,3.5,-3.60822483003176E-15));
#34322=CARTESIAN_POINT('Ctrl Pts',(2.84579300863683,3.5,-1.82072594216369));
#34323=CARTESIAN_POINT('',(0.35420699136317,3.5,-1.82072594216369));
#34324=CARTESIAN_POINT('',(0.,3.5,-1.82072594216369));
#34325=CARTESIAN_POINT('Ctrl Pts',(0.35420699136317,3.5,-1.82072594216369));
#34326=CARTESIAN_POINT('Ctrl Pts',(-0.139184295568601,3.5,3.05311331771918E-15));
#34327=CARTESIAN_POINT('Ctrl Pts',(0.35420699136317,3.5,1.82072594216369));
#34328=CARTESIAN_POINT('Origin',(2.91157561548264,0.,0.));
#34329=CARTESIAN_POINT('',(2.84579300863683,0.173205080756888,3.94145188432738));
#34330=CARTESIAN_POINT('Ctrl Pts',(2.84579300863683,0.173205080756888,3.94145188432738));
#34331=CARTESIAN_POINT('Ctrl Pts',(3.3391842955686,1.75000000000001,3.03108891324553));
#34332=CARTESIAN_POINT('Ctrl Pts',(2.84579300863683,3.32679491924311,2.12072594216369));
#34333=CARTESIAN_POINT('',(2.84579300863683,-0.173205080756887,3.94145188432738));
#34334=CARTESIAN_POINT('Ctrl Pts',(2.84579300863683,-0.173205080756887,
3.94145188432738));
#34335=CARTESIAN_POINT('Ctrl Pts',(2.85025803029788,6.97358837342676E-15,
3.94145188432738));
#34336=CARTESIAN_POINT('Ctrl Pts',(2.84579300863683,0.173205080756888,3.94145188432738));
#34337=CARTESIAN_POINT('',(2.84579300863683,-3.32679491924311,2.12072594216369));
#34338=CARTESIAN_POINT('Ctrl Pts',(2.84579300863683,-3.32679491924311,2.12072594216369));
#34339=CARTESIAN_POINT('Ctrl Pts',(3.3391842955686,-1.75,3.03108891324554));
#34340=CARTESIAN_POINT('Ctrl Pts',(2.84579300863683,-0.173205080756886,
3.94145188432738));
#34341=CARTESIAN_POINT('',(2.84579300863683,-3.5,1.82072594216369));
#34342=CARTESIAN_POINT('Ctrl Pts',(2.84579300863683,-3.5,1.82072594216369));
#34343=CARTESIAN_POINT('Ctrl Pts',(2.85025803029788,-3.41339745962155,1.9707259421637));
#34344=CARTESIAN_POINT('Ctrl Pts',(2.84579300863683,-3.32679491924311,2.12072594216369));
#34345=CARTESIAN_POINT('',(3.10724202769303,-3.5,-5.24027883276575E-16));
#34346=CARTESIAN_POINT('Ctrl Pts',(3.10724202769303,-3.5,-6.19429386851577E-16));
#34347=CARTESIAN_POINT('Ctrl Pts',(3.10724202769303,-3.5,0.855919663339608));
#34348=CARTESIAN_POINT('Ctrl Pts',(2.84579300863683,-3.5,1.82072594216369));
#34349=CARTESIAN_POINT('',(3.2,-3.34203030879952,-4.09280672032477E-16));
#34350=CARTESIAN_POINT('',(2.91157561548264,-3.83322594216369,-4.69434788047936E-16));
#34351=CARTESIAN_POINT('Origin',(3.2,0.,0.));
#34352=CARTESIAN_POINT('',(2.84579300863683,-3.5,-1.82072594216369));
#34353=CARTESIAN_POINT('Ctrl Pts',(2.84579300863683,-3.5,-1.82072594216369));
#34354=CARTESIAN_POINT('Ctrl Pts',(3.10724202769303,-3.5,-0.855919663339607));
#34355=CARTESIAN_POINT('Ctrl Pts',(3.10724202769303,-3.5,-6.19429386851577E-16));
#34356=CARTESIAN_POINT('',(2.84579300863683,-3.32679491924311,-2.12072594216369));
#34357=CARTESIAN_POINT('Ctrl Pts',(2.84579300863683,-3.32679491924311,-2.12072594216369));
#34358=CARTESIAN_POINT('Ctrl Pts',(2.85025803029788,-3.41339745962156,-1.97072594216368));
#34359=CARTESIAN_POINT('Ctrl Pts',(2.84579300863683,-3.5,-1.82072594216369));
#34360=CARTESIAN_POINT('',(2.84579300863683,-0.173205080756888,-3.94145188432738));
#34361=CARTESIAN_POINT('Ctrl Pts',(2.84579300863683,-0.173205080756888,
-3.94145188432738));
#34362=CARTESIAN_POINT('Ctrl Pts',(3.3391842955686,-1.75,-3.03108891324553));
#34363=CARTESIAN_POINT('Ctrl Pts',(2.84579300863683,-3.32679491924311,-2.12072594216369));
#34364=CARTESIAN_POINT('',(2.84579300863683,0.173205080756887,-3.94145188432738));
#34365=CARTESIAN_POINT('Ctrl Pts',(2.84579300863683,0.173205080756887,-3.94145188432738));
#34366=CARTESIAN_POINT('Ctrl Pts',(2.85025803029788,-6.80011602582908E-15,
-3.94145188432738));
#34367=CARTESIAN_POINT('Ctrl Pts',(2.84579300863683,-0.173205080756888,
-3.94145188432738));
#34368=CARTESIAN_POINT('',(2.84579300863683,3.32679491924311,-2.12072594216369));
#34369=CARTESIAN_POINT('Ctrl Pts',(2.84579300863683,3.32679491924311,-2.12072594216369));
#34370=CARTESIAN_POINT('Ctrl Pts',(3.3391842955686,1.74999999999999,-3.03108891324554));
#34371=CARTESIAN_POINT('Ctrl Pts',(2.84579300863683,0.173205080756888,-3.94145188432738));
#34372=CARTESIAN_POINT('Ctrl Pts',(2.84579300863683,3.5,-1.82072594216369));
#34373=CARTESIAN_POINT('Ctrl Pts',(2.85025803029788,3.41339745962155,-1.9707259421637));
#34374=CARTESIAN_POINT('Ctrl Pts',(2.84579300863683,3.32679491924311,-2.12072594216369));
#34375=CARTESIAN_POINT('Origin',(0.1,0.,0.));
#34376=CARTESIAN_POINT('',(0.,2.75545529808154E-16,2.25));
#34377=CARTESIAN_POINT('Origin',(0.,0.,0.));
#34378=CARTESIAN_POINT('',(0.2,-2.51052593825207E-16,2.05));
#34379=CARTESIAN_POINT('',(0.1,2.63299061816681E-16,2.15));
#34380=CARTESIAN_POINT('Origin',(0.2,0.,0.));
#34381=CARTESIAN_POINT('Origin',(0.,0.,0.));
#34382=CARTESIAN_POINT('',(3.,2.51052593825207E-16,2.05));
#34383=CARTESIAN_POINT('',(0.,-2.51052593825207E-16,2.05));
#34384=CARTESIAN_POINT('Origin',(3.,0.,0.));
#34385=CARTESIAN_POINT('Origin',(0.,0.,0.));
#34386=CARTESIAN_POINT('',(0.,-3.34203030879952,4.09280672032477E-16));
#34387=CARTESIAN_POINT('Origin',(0.,0.,0.));
#34388=CARTESIAN_POINT('Origin',(3.1,0.,0.));
#34389=CARTESIAN_POINT('',(3.2,-2.75545529808154E-16,2.25));
#34390=CARTESIAN_POINT('Origin',(3.2,0.,0.));
#34391=CARTESIAN_POINT('',(3.1,-2.63299061816681E-16,2.15));
#34392=CARTESIAN_POINT('Origin',(3.2,0.,0.));
#34393=CARTESIAN_POINT('Origin',(0.,4.5102810375397E-16,3.94145188432738));
#34394=CARTESIAN_POINT('',(0.354206991363169,0.173205080756889,3.94145188432738));
#34395=CARTESIAN_POINT('',(0.,0.173205080756888,3.94145188432738));
#34396=CARTESIAN_POINT('',(0.35420699136317,-0.173205080756887,3.94145188432738));
#34397=CARTESIAN_POINT('Ctrl Pts',(0.354206991363169,0.173205080756889,
3.94145188432738));
#34398=CARTESIAN_POINT('Ctrl Pts',(0.349741969702116,-5.62050406216485E-15,
3.94145188432738));
#34399=CARTESIAN_POINT('Ctrl Pts',(0.35420699136317,-0.173205080756887,
3.94145188432738));
#34400=CARTESIAN_POINT('',(0.,-0.173205080756887,3.94145188432738));
#34401=CARTESIAN_POINT('Origin',(0.,2.47467555702478E-16,4.04145188432738));
#34402=CARTESIAN_POINT('',(0.35420699136317,-3.32679491924311,2.12072594216369));
#34403=CARTESIAN_POINT('Ctrl Pts',(0.35420699136317,-0.173205080756887,
3.94145188432738));
#34404=CARTESIAN_POINT('Ctrl Pts',(-0.139184295568602,-1.75,3.03108891324553));
#34405=CARTESIAN_POINT('Ctrl Pts',(0.35420699136317,-3.32679491924311,2.12072594216369));
#34406=CARTESIAN_POINT('',(0.,-3.32679491924311,2.12072594216369));
#34407=CARTESIAN_POINT('Origin',(0.288424384517358,0.,0.));
#34408=CARTESIAN_POINT('',(0.0927579723069723,-3.5,-5.85970821961734E-16));
#34409=CARTESIAN_POINT('',(0.288424384517358,-3.83322594216369,-4.69434788047936E-16));
#34410=CARTESIAN_POINT('',(0.35420699136317,-3.5,1.82072594216369));
#34411=CARTESIAN_POINT('Ctrl Pts',(0.35420699136317,-3.5,1.82072594216369));
#34412=CARTESIAN_POINT('Ctrl Pts',(0.0927579723069726,-3.5,0.855919663339608));
#34413=CARTESIAN_POINT('Ctrl Pts',(0.0927579723069723,-3.5,-7.43315264221894E-16));
#34414=CARTESIAN_POINT('Ctrl Pts',(0.35420699136317,-3.32679491924311,2.12072594216369));
#34415=CARTESIAN_POINT('Ctrl Pts',(0.349741969702116,-3.41339745962156,
1.97072594216368));
#34416=CARTESIAN_POINT('Ctrl Pts',(0.35420699136317,-3.5,1.82072594216369));
#34417=CARTESIAN_POINT('Ctrl Pts',(0.35420699136317,3.32679491924311,2.12072594216369));
#34418=CARTESIAN_POINT('Ctrl Pts',(-0.139184295568602,1.75,3.03108891324554));
#34419=CARTESIAN_POINT('Ctrl Pts',(0.354206991363169,0.173205080756889,
3.94145188432738));
#34420=CARTESIAN_POINT('',(0.35420699136317,3.32679491924311,-2.12072594216369));
#34421=CARTESIAN_POINT('Ctrl Pts',(0.35420699136317,3.32679491924311,-2.12072594216369));
#34422=CARTESIAN_POINT('Ctrl Pts',(0.349741969702117,3.41339745962156,-1.97072594216369));
#34423=CARTESIAN_POINT('Ctrl Pts',(0.35420699136317,3.5,-1.82072594216369));
#34424=CARTESIAN_POINT('',(0.35420699136317,0.173205080756888,-3.94145188432738));
#34425=CARTESIAN_POINT('Ctrl Pts',(0.35420699136317,0.173205080756887,-3.94145188432738));
#34426=CARTESIAN_POINT('Ctrl Pts',(-0.1391842955686,1.75,-3.03108891324553));
#34427=CARTESIAN_POINT('Ctrl Pts',(0.35420699136317,3.32679491924311,-2.12072594216369));
#34428=CARTESIAN_POINT('',(0.35420699136317,-0.173205080756888,-3.94145188432738));
#34429=CARTESIAN_POINT('Ctrl Pts',(0.35420699136317,-0.173205080756888,
-3.94145188432738));
#34430=CARTESIAN_POINT('Ctrl Pts',(0.349741969702117,6.1409211049579E-15,
-3.94145188432738));
#34431=CARTESIAN_POINT('Ctrl Pts',(0.35420699136317,0.173205080756888,-3.94145188432738));
#34432=CARTESIAN_POINT('',(0.35420699136317,-3.32679491924311,-2.12072594216369));
#34433=CARTESIAN_POINT('Ctrl Pts',(0.35420699136317,-3.32679491924311,-2.12072594216369));
#34434=CARTESIAN_POINT('Ctrl Pts',(-0.139184295568601,-1.75,-3.03108891324554));
#34435=CARTESIAN_POINT('Ctrl Pts',(0.35420699136317,-0.173205080756889,
-3.94145188432738));
#34436=CARTESIAN_POINT('',(0.354206991363169,-3.5,-1.82072594216369));
#34437=CARTESIAN_POINT('Ctrl Pts',(0.354206991363169,-3.5,-1.82072594216369));
#34438=CARTESIAN_POINT('Ctrl Pts',(0.349741969702116,-3.41339745962155,
-1.9707259421637));
#34439=CARTESIAN_POINT('Ctrl Pts',(0.35420699136317,-3.32679491924311,-2.12072594216369));
#34440=CARTESIAN_POINT('Ctrl Pts',(0.0927579723069723,-3.5,-7.43315264221894E-16));
#34441=CARTESIAN_POINT('Ctrl Pts',(0.092757972306972,-3.5,-0.85591966333961));
#34442=CARTESIAN_POINT('Ctrl Pts',(0.354206991363169,-3.5,-1.82072594216369));
#34443=CARTESIAN_POINT('Origin',(0.,-3.41339745962156,1.97072594216369));
#34444=CARTESIAN_POINT('',(0.,-3.5,1.82072594216369));
#34445=CARTESIAN_POINT('Origin',(0.,-3.5,2.02072594216369));
#34446=CARTESIAN_POINT('',(0.,-3.5,-1.82072594216369));
#34447=CARTESIAN_POINT('Origin',(0.,-3.41339745962156,-1.97072594216369));
#34448=CARTESIAN_POINT('',(0.,-3.32679491924311,-2.12072594216369));
#34449=CARTESIAN_POINT('Origin',(0.,3.41339745962155,-1.97072594216369));
#34450=CARTESIAN_POINT('',(0.,3.32679491924311,-2.12072594216369));
#34451=CARTESIAN_POINT('Origin',(0.,-7.42402667107435E-16,-4.04145188432738));
#34452=CARTESIAN_POINT('',(0.,0.173205080756887,-3.94145188432738));
#34453=CARTESIAN_POINT('Origin',(0.,-5.20417042793042E-16,-3.94145188432738));
#34454=CARTESIAN_POINT('',(0.,-0.173205080756888,-3.94145188432738));
#34455=CARTESIAN_POINT('Origin',(0.,-3.5,-2.02072594216369));
#34456=CARTESIAN_POINT('Origin',(0.,3.5,2.02072594216369));
#34457=CARTESIAN_POINT('',(0.,0.,0.));
#34458=CARTESIAN_POINT('Origin',(-3.875,0.,0.));
#34459=CARTESIAN_POINT('',(-7.64010734985006,-1.21647452716103,0.000783377930972141));
#34460=CARTESIAN_POINT('',(-7.70489265014995,-1.21612319654208,0.00132237507692805));
#34461=CARTESIAN_POINT('',(-3.875,-1.215,-1.48794586096403E-16));
#34462=CARTESIAN_POINT('',(-7.785,0.531620960029506,1.09362937143029));
#34463=CARTESIAN_POINT('Ctrl Pts',(-7.64010734985006,-1.21647452716103,
0.000783377930972141));
#34464=CARTESIAN_POINT('Ctrl Pts',(-7.64252235014853,-1.21675455720845,
0.0416081919322704));
#34465=CARTESIAN_POINT('Ctrl Pts',(-7.64493735044699,-1.21487817361819,
0.0824052162368853));
#34466=CARTESIAN_POINT('Ctrl Pts',(-7.64735235074546,-1.21076076162991,
0.122972630877474));
#34467=CARTESIAN_POINT('Ctrl Pts',(-7.67117587831787,-1.17014326021919,
0.523162610914586));
#34468=CARTESIAN_POINT('Ctrl Pts',(-7.69499940589029,-0.911441098580177,
0.901008230831576));
#34469=CARTESIAN_POINT('Ctrl Pts',(-7.7188229334627,-0.553047883833515,
1.08394887030055));
#34470=CARTESIAN_POINT('Ctrl Pts',(-7.7408819556418,-0.221199300582993,
1.25333988979749));
#34471=CARTESIAN_POINT('Ctrl Pts',(-7.7629409778209,0.196119845112543,1.25562826785441));
#34472=CARTESIAN_POINT('Ctrl Pts',(-7.785,0.532258410758873,1.09442686519078));
#34473=CARTESIAN_POINT('',(-7.785,-0.530983509300163,1.09283187766979));
#34474=CARTESIAN_POINT('Origin',(-7.785,0.,0.));
#34475=CARTESIAN_POINT('Ctrl Pts',(-7.785,-0.530983509300162,1.09283187766979));
#34476=CARTESIAN_POINT('Ctrl Pts',(-7.76117647242759,-0.894502226956994,
0.916205949801275));
#34477=CARTESIAN_POINT('Ctrl Pts',(-7.73735294485517,-1.15982398095655,
0.54548974214433));
#34478=CARTESIAN_POINT('Ctrl Pts',(-7.71352941728276,-1.20802527945981,
0.146755193366327));
#34479=CARTESIAN_POINT('Ctrl Pts',(-7.71065049490516,-1.21385010101357,
0.0985706492550221));
#34480=CARTESIAN_POINT('Ctrl Pts',(-7.70777157252755,-1.21650427102171,
0.0499769479485646));
#34481=CARTESIAN_POINT('Ctrl Pts',(-7.70489265014995,-1.21612319654208,
0.00132237507692805));
#34482=CARTESIAN_POINT('Origin',(-3.875,0.,0.));
#34483=CARTESIAN_POINT('',(-7.19010734985006,-1.21334095132918,0.000643174960512083));
#34484=CARTESIAN_POINT('',(-7.25489265014995,-1.21322307873259,0.000540336490138318));
#34485=CARTESIAN_POINT('',(-3.875,-1.215,-1.48794586096403E-16));
#34486=CARTESIAN_POINT('Ctrl Pts',(-7.19010734985006,-1.21334095132918,
0.000643174960512083));
#34487=CARTESIAN_POINT('Ctrl Pts',(-7.19958118471403,-1.21411261089513,
0.161870787822646));
#34488=CARTESIAN_POINT('Ctrl Pts',(-7.209055019578,-1.18425339306602,0.322823852770454));
#34489=CARTESIAN_POINT('Ctrl Pts',(-7.21852885444197,-1.12241826653371,
0.470375966826099));
#34490=CARTESIAN_POINT('Ctrl Pts',(-7.24235238201438,-0.966923594836523,
0.841420206887963));
#34491=CARTESIAN_POINT('Ctrl Pts',(-7.2661759095868,-0.609227870983272,
1.127722949986));
#34492=CARTESIAN_POINT('Ctrl Pts',(-7.28999943715921,-0.213134957863081,
1.19818283107809));
#34493=CARTESIAN_POINT('Ctrl Pts',(-7.31382296473163,0.182957955257111,
1.26864271217017));
#34494=CARTESIAN_POINT('Ctrl Pts',(-7.33764649230405,0.617448057644243,
1.12325973125629));
#34495=CARTESIAN_POINT('Ctrl Pts',(-7.36147001987647,0.89135892310283,0.828592550610321));
#34496=CARTESIAN_POINT('Ctrl Pts',(-7.38529354744888,1.16526978856142,0.533925369964354));
#34497=CARTESIAN_POINT('Ctrl Pts',(-7.40911707502129,1.27860141709146,0.0899739895862994));
#34498=CARTESIAN_POINT('Ctrl Pts',(-7.43294060259371,1.17945999521821,-0.29991955157041));
#34499=CARTESIAN_POINT('Ctrl Pts',(-7.45676413016612,1.08031857334496,-0.689813092727121));
#34500=CARTESIAN_POINT('Ctrl Pts',(-7.48058765773854,0.768704101068424,
-1.02564879466249));
#34501=CARTESIAN_POINT('Ctrl Pts',(-7.50441118531096,0.38730793589725,-1.15370023444288));
#34502=CARTESIAN_POINT('Ctrl Pts',(-7.52823471288338,0.00591177072607862,
-1.28175167422327));
#34503=CARTESIAN_POINT('Ctrl Pts',(-7.55205824045579,-0.445266087339727,
-1.20201885184869));
#34504=CARTESIAN_POINT('Ctrl Pts',(-7.5758817680282,-0.759588595781406,
-0.950885270582782));
#34505=CARTESIAN_POINT('Ctrl Pts',(-7.59729029530215,-1.0420481087287,-0.725209198573965));
#34506=CARTESIAN_POINT('Ctrl Pts',(-7.61869882257611,-1.21399211301332,
-0.361120984795996));
#34507=CARTESIAN_POINT('Ctrl Pts',(-7.64010734985006,-1.21647452716103,
0.000783377930972141));
#34508=CARTESIAN_POINT('Ctrl Pts',(-7.70489265014995,-1.21612319654208,
0.00132237507692805));
#34509=CARTESIAN_POINT('Ctrl Pts',(-7.68394804495514,-1.213350820813,-0.352647161457663));
#34510=CARTESIAN_POINT('Ctrl Pts',(-7.66300343976032,-1.04992940871555,
-0.709838500495367));
#34511=CARTESIAN_POINT('Ctrl Pts',(-7.64205883456551,-0.777998593308031,
-0.936141314006237));
#34512=CARTESIAN_POINT('Ctrl Pts',(-7.61823530699309,-0.468689765646071,
-1.19355038270171));
#34513=CARTESIAN_POINT('Ctrl Pts',(-7.59441177942068,-0.018991267315219,
-1.28161563019358));
#34514=CARTESIAN_POINT('Ctrl Pts',(-7.57058825184826,0.364858107186471,
-1.16089853528955));
#34515=CARTESIAN_POINT('Ctrl Pts',(-7.54676472427585,0.74870748168816,-1.04018144038552));
#34516=CARTESIAN_POINT('Ctrl Pts',(-7.52294119670343,1.06670773236069,-0.710682003085598));
#34517=CARTESIAN_POINT('Ctrl Pts',(-7.49911766913101,1.17338741195235,-0.322840256676906));
#34518=CARTESIAN_POINT('Ctrl Pts',(-7.47529414155859,1.28006709154401,0.0650014897317872));
#34519=CARTESIAN_POINT('Ctrl Pts',(-7.45147061398618,1.1754262000548,0.511185545249247));
#34520=CARTESIAN_POINT('Ctrl Pts',(-7.42764708641377,0.907302988772841,
0.811146645493936));
#34521=CARTESIAN_POINT('Ctrl Pts',(-7.40382355884135,0.639179777490878,
1.11110774573863));
#34522=CARTESIAN_POINT('Ctrl Pts',(-7.38000003126893,0.20757424641616,1.26484589071055));
#34523=CARTESIAN_POINT('Ctrl Pts',(-7.35617650369652,-0.189818330789957,
1.20208175535973));
#34524=CARTESIAN_POINT('Ctrl Pts',(-7.3323529761241,-0.587210907996071,
1.13931762000892));
#34525=CARTESIAN_POINT('Ctrl Pts',(-7.30852944855169,-0.950390531333583,
0.860051204335379));
#34526=CARTESIAN_POINT('Ctrl Pts',(-7.28470592097928,-1.11306298319363,
0.492106025130156));
#34527=CARTESIAN_POINT('Ctrl Pts',(-7.27476816403617,-1.18092024249372,
0.338621208567414));
#34528=CARTESIAN_POINT('Ctrl Pts',(-7.26483040709306,-1.2138880203146,0.169705741544439));
#34529=CARTESIAN_POINT('Ctrl Pts',(-7.25489265014995,-1.21322307873259,
0.000540336490138318));
#34530=CARTESIAN_POINT('Origin',(-3.875,0.,0.));
#34531=CARTESIAN_POINT('',(-6.74010734985006,-1.21414526361761,-0.00102520398183079));
#34532=CARTESIAN_POINT('',(-6.80489265014995,-1.21436027551958,-0.00106957681048473));
#34533=CARTESIAN_POINT('',(-3.875,-1.215,-1.48794586096403E-16));
#34534=CARTESIAN_POINT('Ctrl Pts',(-6.74010734985006,-1.21414526361761,
-0.00102520398183079));
#34535=CARTESIAN_POINT('Ctrl Pts',(-6.75664001927953,-1.21189888768043,
0.279861953419163));
#34536=CARTESIAN_POINT('Ctrl Pts',(-6.77317268870901,-1.11490370551602,
0.562149070738359));
#34537=CARTESIAN_POINT('Ctrl Pts',(-6.78970535813848,-0.936647874117358,
0.777023963888983));
#34538=CARTESIAN_POINT('Ctrl Pts',(-6.8135288857109,-0.679781750205209,
1.08665804708595));
#34539=CARTESIAN_POINT('Ctrl Pts',(-6.83735241328332,-0.254180127287122,
1.25631250433391));
#34540=CARTESIAN_POINT('Ctrl Pts',(-6.86117594085573,0.145254223191172,
1.20829487101183));
#34541=CARTESIAN_POINT('Ctrl Pts',(-6.88499946842815,0.544688573669464,
1.16027723768975));
#34542=CARTESIAN_POINT('Ctrl Pts',(-6.90882299600056,0.917955651707963,
0.894587513797618));
#34543=CARTESIAN_POINT('Ctrl Pts',(-6.93264652357298,1.0941190081907,0.532896993842244));
#34544=CARTESIAN_POINT('Ctrl Pts',(-6.95647005114539,1.27028236467343,0.171206473886867));
#34545=CARTESIAN_POINT('Ctrl Pts',(-6.98029357871781,1.2493419996004,-0.286484842131756));
#34546=CARTESIAN_POINT('Ctrl Pts',(-7.00411710629023,1.04088761013505,-0.630578012028203));
#34547=CARTESIAN_POINT('Ctrl Pts',(-7.02794063386264,0.832433220669708,
-0.97467118192465));
#34548=CARTESIAN_POINT('Ctrl Pts',(-7.05176416143506,0.436464806812055,
-1.20516620569892));
#34549=CARTESIAN_POINT('Ctrl Pts',(-7.07558768900747,0.0343145048386373,
-1.21651013722172));
#34550=CARTESIAN_POINT('Ctrl Pts',(-7.09941121657989,-0.36783579713478,
-1.22785406874451));
#34551=CARTESIAN_POINT('Ctrl Pts',(-7.1232347441523,-0.776167987223963,
-1.02004690801583));
#34552=CARTESIAN_POINT('Ctrl Pts',(-7.14705827172472,-1.00368727249799,
-0.688250459138645));
#34553=CARTESIAN_POINT('Ctrl Pts',(-7.16140796443317,-1.14072960676204,
-0.488398566144665));
#34554=CARTESIAN_POINT('Ctrl Pts',(-7.17575765714162,-1.21217214505317,
-0.243562760007505));
#34555=CARTESIAN_POINT('Ctrl Pts',(-7.19010734985006,-1.21334095132918,
0.000643174960512083));
#34556=CARTESIAN_POINT('Ctrl Pts',(-7.25489265014995,-1.21322307873259,
0.000540336490138318));
#34557=CARTESIAN_POINT('Ctrl Pts',(-7.24100687952064,-1.21229397306592,
-0.235830106704008));
#34558=CARTESIAN_POINT('Ctrl Pts',(-7.22712110889133,-1.14570118758852,
-0.472688522656612));
#34559=CARTESIAN_POINT('Ctrl Pts',(-7.21323533826202,-1.01687317306236,
-0.668621881745882));
#34560=CARTESIAN_POINT('Ctrl Pts',(-7.18941181068961,-0.795845630688474,
-1.0047806666798));
#34561=CARTESIAN_POINT('Ctrl Pts',(-7.1655882831172,-0.391625265558127,
-1.22047429381071));
#34562=CARTESIAN_POINT('Ctrl Pts',(-7.14176475554478,0.0106703029332755,
-1.21694480617947));
#34563=CARTESIAN_POINT('Ctrl Pts',(-7.11794122797236,0.412965871424674,
-1.21341531854822));
#34564=CARTESIAN_POINT('Ctrl Pts',(-7.09411770039994,0.81333664327713,-0.99066271615481));
#34565=CARTESIAN_POINT('Ctrl Pts',(-7.07029417282752,1.02843750508761,-0.650686201737506));
#34566=CARTESIAN_POINT('Ctrl Pts',(-7.04647064525511,1.24353836689809,-0.310709687320199));
#34567=CARTESIAN_POINT('Ctrl Pts',(-7.0226471176827,1.27336931866659,0.146490739121003));
#34568=CARTESIAN_POINT('Ctrl Pts',(-6.99882359011028,1.10426763327177,0.511536654314946));
#34569=CARTESIAN_POINT('Ctrl Pts',(-6.97500006253787,0.935165947876942,
0.876582569508885));
#34570=CARTESIAN_POINT('Ctrl Pts',(-6.95117653496545,0.567131625318796,
1.14947397345556));
#34571=CARTESIAN_POINT('Ctrl Pts',(-6.92735300739304,0.168705643738918,
1.20524384305627));
#34572=CARTESIAN_POINT('Ctrl Pts',(-6.90352947982062,-0.229720337840963,
1.26101371265697));
#34573=CARTESIAN_POINT('Ctrl Pts',(-6.87970595224821,-0.658537978442577,
1.09966204791169));
#34574=CARTESIAN_POINT('Ctrl Pts',(-6.85588242467579,-0.92137219093613,
0.795077889353162));
#34575=CARTESIAN_POINT('Ctrl Pts',(-6.83888583316718,-1.10888790332011,
0.577776211116059));
#34576=CARTESIAN_POINT('Ctrl Pts',(-6.82188924165856,-1.21191926571901,
0.287570241923624));
#34577=CARTESIAN_POINT('Ctrl Pts',(-6.80489265014995,-1.21436027551958,
-0.00106957681048473));
#34578=CARTESIAN_POINT('Origin',(-3.875,0.,0.));
#34579=CARTESIAN_POINT('',(-6.29010734985006,-1.21698889981248,-7.32665095025398E-5));
#34580=CARTESIAN_POINT('',(-6.35489265014995,-1.21698887272922,7.32242133118944E-5));
#34581=CARTESIAN_POINT('',(-3.875,-1.215,-1.48794586096403E-16));
#34582=CARTESIAN_POINT('Ctrl Pts',(-6.29010734985006,-1.21698889981248,
-7.32665095025398E-5));
#34583=CARTESIAN_POINT('Ctrl Pts',(-6.31369885384504,-1.21664139445038,
0.398323610426177));
#34584=CARTESIAN_POINT('Ctrl Pts',(-6.33729035784002,-1.00225596389633,
0.7970411536321));
#34585=CARTESIAN_POINT('Ctrl Pts',(-6.360881861835,-0.669584224757944,1.01623442508117));
#34586=CARTESIAN_POINT('Ctrl Pts',(-6.38470538940741,-0.333640643051026,
1.23758347290643));
#34587=CARTESIAN_POINT('Ctrl Pts',(-6.40852891697983,0.12292739193656,1.27585962421094));
#34588=CARTESIAN_POINT('Ctrl Pts',(-6.43235244455225,0.49103611136388,1.11353445102204));
#34589=CARTESIAN_POINT('Ctrl Pts',(-6.45617597212467,0.859144830791203,
0.951209277833139));
#34590=CARTESIAN_POINT('Ctrl Pts',(-6.47999949969708,1.13879423465826,0.588282780150836));
#34591=CARTESIAN_POINT('Ctrl Pts',(-6.5038230272695,1.20191983375759,0.190955897270189));
#34592=CARTESIAN_POINT('Ctrl Pts',(-6.52764655484191,1.26504543285693,-0.206370985610454));
#34593=CARTESIAN_POINT('Ctrl Pts',(-6.55147008241433,1.11164722718855,-0.638098253689441));
#34594=CARTESIAN_POINT('Ctrl Pts',(-6.57529360998674,0.811973402978483,
-0.906517865129097));
#34595=CARTESIAN_POINT('Ctrl Pts',(-6.59911713755915,0.512299578768414,
-1.17493747656875));
#34596=CARTESIAN_POINT('Ctrl Pts',(-6.62294066513157,0.0663501360166598,
-1.28004943136908));
#34597=CARTESIAN_POINT('Ctrl Pts',(-6.64676419270399,-0.321653908877025,
-1.17371810067433));
#34598=CARTESIAN_POINT('Ctrl Pts',(-6.67058772027641,-0.709657953770708,
-1.06738676997957));
#34599=CARTESIAN_POINT('Ctrl Pts',(-6.69441124784882,-1.03971660080632,
-0.749612153789738));
#34600=CARTESIAN_POINT('Ctrl Pts',(-6.71823477542124,-1.16068061187102,
-0.36591799112184));
#34601=CARTESIAN_POINT('Ctrl Pts',(-6.72552563356418,-1.19769995933722,
-0.24849374730308));
#34602=CARTESIAN_POINT('Ctrl Pts',(-6.73281649170712,-1.21513590873778,
-0.124895606612254));
#34603=CARTESIAN_POINT('Ctrl Pts',(-6.74010734985006,-1.21414526361761,
-0.00102520398183079));
#34604=CARTESIAN_POINT('Ctrl Pts',(-6.80489265014995,-1.21436027551958,
-0.00106957681048473));
#34605=CARTESIAN_POINT('Ctrl Pts',(-6.79806571408614,-1.21534074374059,
-0.117006091903337));
#34606=CARTESIAN_POINT('Ctrl Pts',(-6.79123877802234,-1.20009248969292,
-0.232689932458696));
#34607=CARTESIAN_POINT('Ctrl Pts',(-6.78441184195854,-1.1675718035762,-0.343295225079648));
#34608=CARTESIAN_POINT('Ctrl Pts',(-6.76058831438612,-1.05408641933721,
-0.729267528582172));
#34609=CARTESIAN_POINT('Ctrl Pts',(-6.73676478681371,-0.730264866473754,
-1.05339548321545));
#34610=CARTESIAN_POINT('Ctrl Pts',(-6.71294125924129,-0.344400251683041,
-1.16724619030599));
#34611=CARTESIAN_POINT('Ctrl Pts',(-6.68911773166888,0.0414643631076694,
-1.28109689739654));
#34612=CARTESIAN_POINT('Ctrl Pts',(-6.66529420409646,0.489372039825632,
-1.18467035694436));
#34613=CARTESIAN_POINT('Ctrl Pts',(-6.64147067652405,0.79420506113041,-0.922124568184181));
#34614=CARTESIAN_POINT('Ctrl Pts',(-6.61764714895163,1.09903808243519,-0.659578779423996));
#34615=CARTESIAN_POINT('Ctrl Pts',(-6.59382362137922,1.26079644832678,-0.230913742355804));
#34616=CARTESIAN_POINT('Ctrl Pts',(-6.5700000938068,1.20540343124301,0.167564747811473));
#34617=CARTESIAN_POINT('Ctrl Pts',(-6.54617656623438,1.15001041415923,0.566043237978747));
#34618=CARTESIAN_POINT('Ctrl Pts',(-6.52235303866197,0.877466014100086,
0.934335181245106));
#34619=CARTESIAN_POINT('Ctrl Pts',(-6.49852951108955,0.512581026296972,
1.10378259911935));
#34620=CARTESIAN_POINT('Ctrl Pts',(-6.47470598351713,0.147696038493855,
1.27323001699359));
#34621=CARTESIAN_POINT('Ctrl Pts',(-6.45088245594472,-0.309529537053229,
1.24383290947571));
#34622=CARTESIAN_POINT('Ctrl Pts',(-6.4270589283723,-0.649710822647686,
1.02905355139116));
#34623=CARTESIAN_POINT('Ctrl Pts',(-6.40323540079989,-0.989892108242138,
0.814274193306606));
#34624=CARTESIAN_POINT('Ctrl Pts',(-6.37941187322747,-1.21302910388396,
0.414112584655379));
#34625=CARTESIAN_POINT('Ctrl Pts',(-6.35558834565506,-1.21693698036283,
0.0118213808785433));
#34626=CARTESIAN_POINT('Ctrl Pts',(-6.35535644715336,-1.21697501967911,
0.00790547349998427));
#34627=CARTESIAN_POINT('Ctrl Pts',(-6.35512454865165,-1.21699228681968,
0.00398936434018253));
#34628=CARTESIAN_POINT('Ctrl Pts',(-6.35489265014995,-1.21698887272922,
7.32242133118944E-5));
#34629=CARTESIAN_POINT('Origin',(-3.875,0.,0.));
#34630=CARTESIAN_POINT('',(-5.84010734985006,-1.21436037857631,0.00106961527518802));
#34631=CARTESIAN_POINT('',(-5.90489265014995,-1.2141452873099,0.00102522403285088));
#34632=CARTESIAN_POINT('',(-3.875,-1.215,-1.48794586096403E-16));
#34633=CARTESIAN_POINT('Ctrl Pts',(-5.84010734985006,-1.21436037857631,
0.00106961527518802));
#34634=CARTESIAN_POINT('Ctrl Pts',(-5.84693416083814,-1.21534082109932,
0.117003935709098));
#34635=CARTESIAN_POINT('Ctrl Pts',(-5.85376097182621,-1.2000931166481,0.232685591943789));
#34636=CARTESIAN_POINT('Ctrl Pts',(-5.86058778281428,-1.16757359504631,
0.343289003077695));
#34637=CARTESIAN_POINT('Ctrl Pts',(-5.88441131038669,-1.05409019542155,
0.729261812249731));
#34638=CARTESIAN_POINT('Ctrl Pts',(-5.9082348379591,-0.730270408341806,
1.05339169431114));
#34639=CARTESIAN_POINT('Ctrl Pts',(-5.93205836553151,-0.344406397450761,
1.16724447863947));
#34640=CARTESIAN_POINT('Ctrl Pts',(-5.95588189310393,0.0414576134402811,
1.28109726296781));
#34641=CARTESIAN_POINT('Ctrl Pts',(-5.97970542067635,0.489365848142625,
1.18467294956306));
#34642=CARTESIAN_POINT('Ctrl Pts',(-6.00352894824877,0.794200262982349,
0.922128722957946));
#34643=CARTESIAN_POINT('Ctrl Pts',(-6.02735247582118,1.09903467782208,0.659584496352827));
#34644=CARTESIAN_POINT('Ctrl Pts',(-6.0511760033936,1.26079527279918,0.230920356547328));
#34645=CARTESIAN_POINT('Ctrl Pts',(-6.07499953096601,1.20540433683121,-0.167558420373342));
#34646=CARTESIAN_POINT('Ctrl Pts',(-6.09882305853843,1.15001340086323,-0.56603719729401));
#34647=CARTESIAN_POINT('Ctrl Pts',(-6.12264658611084,0.877470933950182,
-0.934330611329849));
#34648=CARTESIAN_POINT('Ctrl Pts',(-6.14647011368326,0.512586826446446,
-1.10377995318354));
#34649=CARTESIAN_POINT('Ctrl Pts',(-6.17029364125568,0.147702718942707,
-1.27322929503724));
#34650=CARTESIAN_POINT('Ctrl Pts',(-6.19411716882809,-0.30952302915172,
-1.24383456470878));
#34651=CARTESIAN_POINT('Ctrl Pts',(-6.21794069640051,-0.64970545087747,
-1.02905697905386));
#34652=CARTESIAN_POINT('Ctrl Pts',(-6.24176422397292,-0.98988787260322,
-0.814279393398937));
#34653=CARTESIAN_POINT('Ctrl Pts',(-6.26558775154534,-1.21302696796029,
-0.414118952417547));
#34654=CARTESIAN_POINT('Ctrl Pts',(-6.28941127911776,-1.2169369514257,-0.0118277597538365));
#34655=CARTESIAN_POINT('Ctrl Pts',(-6.28964330269519,-1.21697503177919,
-0.00790974041732449));
#34656=CARTESIAN_POINT('Ctrl Pts',(-6.28987532627263,-1.21699231754445,
-0.00399151897214472));
#34657=CARTESIAN_POINT('Ctrl Pts',(-6.29010734985006,-1.21698889981248,
-7.32665095025398E-5));
#34658=CARTESIAN_POINT('Ctrl Pts',(-6.35489265014995,-1.21698887272922,
7.32242133118944E-5));
#34659=CARTESIAN_POINT('Ctrl Pts',(-6.33130102107924,-1.21664154855489,
-0.3983257502674));
#34660=CARTESIAN_POINT('Ctrl Pts',(-6.30770939200853,-1.00225352412178,
-0.79704521887662));
#34661=CARTESIAN_POINT('Ctrl Pts',(-6.28411776293781,-0.669578881611528,
-1.01623790290697));
#34662=CARTESIAN_POINT('Ctrl Pts',(-6.2602942353654,-0.333634149065464,
-1.2375851840132));
#34663=CARTESIAN_POINT('Ctrl Pts',(-6.23647070779298,0.122934073342565,
-1.2758589473232));
#34664=CARTESIAN_POINT('Ctrl Pts',(-6.21264718022056,0.491041931694761,
-1.11353184948667));
#34665=CARTESIAN_POINT('Ctrl Pts',(-6.18882365264814,0.859149790046959,
-0.951204751650141));
#34666=CARTESIAN_POINT('Ctrl Pts',(-6.16500012507573,1.13879728434332,-0.588276792667072));
#34667=CARTESIAN_POINT('Ctrl Pts',(-6.14117659750332,1.20192080050794,-0.190949592008526));
#34668=CARTESIAN_POINT('Ctrl Pts',(-6.1173530699309,1.26504431667255,0.206377608650018));
#34669=CARTESIAN_POINT('Ctrl Pts',(-6.09352954235848,1.11164385470542,0.638104050984041));
#34670=CARTESIAN_POINT('Ctrl Pts',(-6.06970601478607,0.811968631768357,
0.906522088974185));
#34671=CARTESIAN_POINT('Ctrl Pts',(-6.04588248721365,0.512293408831295,
1.17494012696433));
#34672=CARTESIAN_POINT('Ctrl Pts',(-6.02205895964123,0.066343424924305,
1.2800497606106));
#34673=CARTESIAN_POINT('Ctrl Pts',(-5.99823543206882,-0.321660050735999,
1.17371639214635));
#34674=CARTESIAN_POINT('Ctrl Pts',(-5.9744119044964,-0.709663526396303,
1.06738302368211));
#34675=CARTESIAN_POINT('Ctrl Pts',(-5.95058837692399,-1.03972049380992,
0.749606653107353));
#34676=CARTESIAN_POINT('Ctrl Pts',(-5.92676484935158,-1.16068249382993,
0.365911882482422));
#34677=CARTESIAN_POINT('Ctrl Pts',(-5.91947411628437,-1.19770059078224,
0.24848946704008));
#34678=CARTESIAN_POINT('Ctrl Pts',(-5.91218338321716,-1.21513593053589,
0.124893473920583));
#34679=CARTESIAN_POINT('Ctrl Pts',(-5.90489265014995,-1.2141452873099,0.00102522403285088));
#34680=CARTESIAN_POINT('Origin',(-3.875,0.,0.));
#34681=CARTESIAN_POINT('',(-5.39010734985006,-1.21322636163708,-0.000530816515116744));
#34682=CARTESIAN_POINT('',(-5.45489265014995,-1.21334113603808,-0.000641635778683531));
#34683=CARTESIAN_POINT('',(-3.875,-1.215,-1.48794586096403E-16));
#34684=CARTESIAN_POINT('Ctrl Pts',(-5.39010734985006,-1.21322636163708,
-0.000530816515116744));
#34685=CARTESIAN_POINT('Ctrl Pts',(-5.40399299540364,-1.21229583382079,
0.235833215312909));
#34686=CARTESIAN_POINT('Ctrl Pts',(-5.41787864095721,-1.14570162521325,
0.472681662538362));
#34687=CARTESIAN_POINT('Ctrl Pts',(-5.43176428651079,-1.01687485630836,
0.668611221932072));
#34688=CARTESIAN_POINT('Ctrl Pts',(-5.4555878140832,-0.79584746012218,1.00476651571784));
#34689=CARTESIAN_POINT('Ctrl Pts',(-5.47941134165562,-0.391631796683574,
1.22047264070872));
#34690=CARTESIAN_POINT('Ctrl Pts',(-5.50323486922803,0.0106629538454742,
1.21694771494172));
#34691=CARTESIAN_POINT('Ctrl Pts',(-5.52705839680045,0.412957704374528,
1.21342278917472));
#34692=CARTESIAN_POINT('Ctrl Pts',(-5.55088192437287,0.813331541994021,
0.990666812649834));
#34693=CARTESIAN_POINT('Ctrl Pts',(-5.57470545194528,1.02843463753263,0.65069012272196));
#34694=CARTESIAN_POINT('Ctrl Pts',(-5.5985289795177,1.24353773307125,0.310713432794086));
#34695=CARTESIAN_POINT('Ctrl Pts',(-5.6223525070901,1.27337008652897,-0.146483970536773));
#34696=CARTESIAN_POINT('Ctrl Pts',(-5.64617603466252,1.10427007370218,-0.51153010059119));
#34697=CARTESIAN_POINT('Ctrl Pts',(-5.66999956223494,0.935170060875382,
-0.876576230645603));
#34698=CARTESIAN_POINT('Ctrl Pts',(-5.69382308980737,0.567137681764061,
-1.14947108742358));
#34699=CARTESIAN_POINT('Ctrl Pts',(-5.71764661737978,0.168712105264506,
-1.20524340488892));
#34700=CARTESIAN_POINT('Ctrl Pts',(-5.7414701449522,-0.229713471235052,
-1.26101572235425));
#34701=CARTESIAN_POINT('Ctrl Pts',(-5.7652936725246,-0.658532245122845,
-1.09966550050696));
#34702=CARTESIAN_POINT('Ctrl Pts',(-5.78911720009702,-0.921368125981851,
-0.795082521441981));
#34703=CARTESIAN_POINT('Ctrl Pts',(-5.80611391668136,-1.10888640855265,
-0.57778008561055));
#34704=CARTESIAN_POINT('Ctrl Pts',(-5.82311063326571,-1.21191937007028,
-0.287572151760318));
#34705=CARTESIAN_POINT('Ctrl Pts',(-5.84010734985006,-1.21436037857631,
0.00106961527518802));
#34706=CARTESIAN_POINT('Ctrl Pts',(-5.90489265014995,-1.2141452873099,0.00102522403285088));
#34707=CARTESIAN_POINT('Ctrl Pts',(-5.88835985564474,-1.21189886013553,
-0.27986399550588));
#34708=CARTESIAN_POINT('Ctrl Pts',(-5.87182706113953,-1.11490208679248,
-0.562153217588061));
#34709=CARTESIAN_POINT('Ctrl Pts',(-5.85529426663433,-0.936643782657277,
-0.777028816434906));
#34710=CARTESIAN_POINT('Ctrl Pts',(-5.83147073906191,-0.6797760388382,-1.08666157405219));
#34711=CARTESIAN_POINT('Ctrl Pts',(-5.8076472114895,-0.254173518573637,
-1.25631391861166));
#34712=CARTESIAN_POINT('Ctrl Pts',(-5.78382368391708,0.145260560092642,
-1.20829413924618));
#34713=CARTESIAN_POINT('Ctrl Pts',(-5.76000015634467,0.544694638758927,
-1.16027435988069));
#34714=CARTESIAN_POINT('Ctrl Pts',(-5.73617662877225,0.91796027582693,-0.894582456590248));
#34715=CARTESIAN_POINT('Ctrl Pts',(-5.71235310119983,1.0941217498074,-0.532891127546195));
#34716=CARTESIAN_POINT('Ctrl Pts',(-5.68852957362741,1.27028322378787,-0.171199798502151));
#34717=CARTESIAN_POINT('Ctrl Pts',(-5.664706046055,1.24934053468083,0.286490956295504));
#34718=CARTESIAN_POINT('Ctrl Pts',(-5.64088251848259,1.04088431532232,0.630583221573055));
#34719=CARTESIAN_POINT('Ctrl Pts',(-5.61705899091017,0.832428095963802,
0.974675486850615));
#34720=CARTESIAN_POINT('Ctrl Pts',(-5.59323546333775,0.436458346353827,
1.20516926260807));
#34721=CARTESIAN_POINT('Ctrl Pts',(-5.56941193576534,0.0343080586227004,
1.21651071279303));
#34722=CARTESIAN_POINT('Ctrl Pts',(-5.54558840819292,-0.36784222910842,
1.22785216297799));
#34723=CARTESIAN_POINT('Ctrl Pts',(-5.52176488062051,-0.776173054960685,
1.02004128759047));
#34724=CARTESIAN_POINT('Ctrl Pts',(-5.49794135304809,-1.00369071422132,
0.68824436605509));
#34725=CARTESIAN_POINT('Ctrl Pts',(-5.48359178541538,-1.14073087459529,
0.488393930328221));
#34726=CARTESIAN_POINT('Ctrl Pts',(-5.46924221778267,-1.21217228758971,
0.243561541831228));
#34727=CARTESIAN_POINT('Ctrl Pts',(-5.45489265014995,-1.21334113603808,
-0.000641635778683531));
#34728=CARTESIAN_POINT('Origin',(-3.875,0.,0.));
#34729=CARTESIAN_POINT('',(-4.94010734985006,-1.21630354408558,-0.000802320355120511));
#34730=CARTESIAN_POINT('',(-5.00489265014995,-1.21648875695904,-0.000697868307776));
#34731=CARTESIAN_POINT('',(-3.875,-1.215,-1.48794586096403E-16));
#34732=CARTESIAN_POINT('Ctrl Pts',(-4.94010734985006,-1.21630354408558,
-0.000802320355120511));
#34733=CARTESIAN_POINT('Ctrl Pts',(-4.96105182996914,-1.21360198855398,
0.353421363843449));
#34734=CARTESIAN_POINT('Ctrl Pts',(-4.98199631008822,-1.0499189859206,0.709819131320941));
#34735=CARTESIAN_POINT('Ctrl Pts',(-5.00294079020731,-0.777920094248849,
0.935903716441848));
#34736=CARTESIAN_POINT('Ctrl Pts',(-5.02676431777972,-0.468531985374048,
1.19306609606182));
#34737=CARTESIAN_POINT('Ctrl Pts',(-5.05058784535213,-0.0190029011941928,
1.28162702087502));
#34738=CARTESIAN_POINT('Ctrl Pts',(-5.07441137292455,0.36480685212754,1.16103031834945));
#34739=CARTESIAN_POINT('Ctrl Pts',(-5.09823490049697,0.748616605449275,
1.04043361582388));
#34740=CARTESIAN_POINT('Ctrl Pts',(-5.12205842806939,1.06670702791289,0.710679285959532));
#34741=CARTESIAN_POINT('Ctrl Pts',(-5.1458819556418,1.17340969880785,0.322777195956391));
#34742=CARTESIAN_POINT('Ctrl Pts',(-5.16970548321422,1.28011236970281,-0.0651248940467475));
#34743=CARTESIAN_POINT('Ctrl Pts',(-5.19352901078663,1.17542728902912,-0.511174744188683));
#34744=CARTESIAN_POINT('Ctrl Pts',(-5.21735253835905,0.907294631330801,
-0.811105351630773));
#34745=CARTESIAN_POINT('Ctrl Pts',(-5.24117606593146,0.639161973632482,
-1.11103595907287));
#34746=CARTESIAN_POINT('Ctrl Pts',(-5.26499959350388,0.207581738909531,
-1.26484732381511));
#34747=CARTESIAN_POINT('Ctrl Pts',(-5.28882312107629,-0.18980538087671,
-1.20210205759585));
#34748=CARTESIAN_POINT('Ctrl Pts',(-5.31264664864871,-0.587192500662953,
-1.13935679137658));
#34749=CARTESIAN_POINT('Ctrl Pts',(-5.33647017622113,-0.950386505512486,
-0.860054894195808));
#34750=CARTESIAN_POINT('Ctrl Pts',(-5.36029370379354,-1.11306394347038,
-0.492101714315088));
#34751=CARTESIAN_POINT('Ctrl Pts',(-5.37023158581238,-1.18092413674523,
-0.338611628558619));
#34752=CARTESIAN_POINT('Ctrl Pts',(-5.38016946783122,-1.21389233540243,
-0.169695285876029));
#34753=CARTESIAN_POINT('Ctrl Pts',(-5.39010734985006,-1.21322636163708,
-0.000530816515116744));
#34754=CARTESIAN_POINT('Ctrl Pts',(-5.45489265014995,-1.21334113603808,
-0.000641635778683531));
#34755=CARTESIAN_POINT('Ctrl Pts',(-5.44541869021025,-1.21411284036108,
-0.161870962058142));
#34756=CARTESIAN_POINT('Ctrl Pts',(-5.43594473027055,-1.1842528333953,-0.322826016203698));
#34757=CARTESIAN_POINT('Ctrl Pts',(-5.42647077033085,-1.12241602959814,
-0.470380286280767));
#34758=CARTESIAN_POINT('Ctrl Pts',(-5.40264724275843,-0.966919193045314,
-0.841425049398009));
#34759=CARTESIAN_POINT('Ctrl Pts',(-5.37882371518601,-0.609221027270653,
-1.12773160794927));
#34760=CARTESIAN_POINT('Ctrl Pts',(-5.3550001876136,-0.21312818352657,-1.19818685296113));
#34761=CARTESIAN_POINT('Ctrl Pts',(-5.33117666004118,0.182964660217511,
-1.268642097973));
#34762=CARTESIAN_POINT('Ctrl Pts',(-5.30735313246877,0.617452181931014,
-1.12324602944548));
#34763=CARTESIAN_POINT('Ctrl Pts',(-5.28352960489635,0.891362307521405,
-0.828582279530157));
#34764=CARTESIAN_POINT('Ctrl Pts',(-5.25970607732393,1.1652724331118,-0.533918529614831));
#34765=CARTESIAN_POINT('Ctrl Pts',(-5.23588254975151,1.27860516257908,-0.0899870983117007));
#34766=CARTESIAN_POINT('Ctrl Pts',(-5.2120590221791,1.17946016019986,0.299915134200719));
#34767=CARTESIAN_POINT('Ctrl Pts',(-5.18823549460669,1.08031515782065,0.689817366713137));
#34768=CARTESIAN_POINT('Ctrl Pts',(-5.16441196703427,0.76869242359494,1.02569040043484));
#34769=CARTESIAN_POINT('Ctrl Pts',(-5.14058843946186,0.387298522532,1.15372232866756));
#34770=CARTESIAN_POINT('Ctrl Pts',(-5.11676491188944,0.00590462146906182,
1.28175425690027));
#34771=CARTESIAN_POINT('Ctrl Pts',(-5.09294138431702,-0.445260446431109,
1.20194507964399));
#34772=CARTESIAN_POINT('Ctrl Pts',(-5.0691178567446,-0.759587181857625,
0.950843136578795));
#34773=CARTESIAN_POINT('Ctrl Pts',(-5.04770945454638,-1.0420488430541,0.725196813902441));
#34774=CARTESIAN_POINT('Ctrl Pts',(-5.02630105234817,-1.21401002870781,
0.361227173945358));
#34775=CARTESIAN_POINT('Ctrl Pts',(-5.00489265014995,-1.21648875695904,
-0.000697868307776));
#34776=CARTESIAN_POINT('Origin',(-3.875,0.,0.));
#34777=CARTESIAN_POINT('',(-4.49010734985006,-1.21569869268569,0.00101898845098317));
#34778=CARTESIAN_POINT('',(-4.55489265014995,-1.21546413760631,0.00106646674887225));
#34779=CARTESIAN_POINT('',(-3.875,-1.215,-1.48794586096403E-16));
#34780=CARTESIAN_POINT('Ctrl Pts',(-4.49010734985006,-1.21569869268569,
0.00101898845098317));
#34781=CARTESIAN_POINT('Ctrl Pts',(-4.49428713696223,-1.21633390645148,
0.0718012148764551));
#34782=CARTESIAN_POINT('Ctrl Pts',(-4.4984669240744,-1.21068428894374,0.142482134878694));
#34783=CARTESIAN_POINT('Ctrl Pts',(-4.50264671118658,-1.19838922396478,
0.211987517016677));
#34784=CARTESIAN_POINT('Ctrl Pts',(-4.52647023875899,-1.12831105690268,
0.608147259931254));
#34785=CARTESIAN_POINT('Ctrl Pts',(-4.55029376633141,-0.842345119511607,
0.966117813998743));
#34786=CARTESIAN_POINT('Ctrl Pts',(-4.57411729390382,-0.471448534467992,
1.12196778867924));
#34787=CARTESIAN_POINT('Ctrl Pts',(-4.59794082147624,-0.100551949424372,
1.27781776335974));
#34788=CARTESIAN_POINT('Ctrl Pts',(-4.62176434904865,0.355275283271792,
1.23154715865325));
#34789=CARTESIAN_POINT('Ctrl Pts',(-4.64558787662107,0.68728864189162,1.00434543968327));
#34790=CARTESIAN_POINT('Ctrl Pts',(-4.66941140419349,1.01930200051144,0.777143720713295));
#34791=CARTESIAN_POINT('Ctrl Pts',(-4.6932349317659,1.22750148505493,0.369010887479842));
#34792=CARTESIAN_POINT('Ctrl Pts',(-4.71705845933832,1.21654285387123,-0.0331500253492225));
#34793=CARTESIAN_POINT('Ctrl Pts',(-4.74088198691073,1.20558422268752,-0.435310938178298));
#34794=CARTESIAN_POINT('Ctrl Pts',(-4.76470551448314,0.9754674757766,-0.831499930602986));
#34795=CARTESIAN_POINT('Ctrl Pts',(-4.78852904205556,0.63157379010677,-1.04028360899131));
#34796=CARTESIAN_POINT('Ctrl Pts',(-4.81235256962798,0.287680104436951,
-1.24906728737962));
#34797=CARTESIAN_POINT('Ctrl Pts',(-4.83617609720039,-0.169990519991771,
-1.27044565173157));
#34798=CARTESIAN_POINT('Ctrl Pts',(-4.85999962477281,-0.531849386513239,
-1.09462855323224));
#34799=CARTESIAN_POINT('Ctrl Pts',(-4.88382315234523,-0.893708253034712,
-0.918811454732897));
#34800=CARTESIAN_POINT('Ctrl Pts',(-4.90764667991764,-1.15975536164893,
-0.545798893382257));
#34801=CARTESIAN_POINT('Ctrl Pts',(-4.93147020749006,-1.20815534917116,
-0.146410695493564));
#34802=CARTESIAN_POINT('Ctrl Pts',(-4.93434925494339,-1.21400443513854,
-0.0981450652031645));
#34803=CARTESIAN_POINT('Ctrl Pts',(-4.93722830239672,-1.21667490238758,
-0.0494942329786094));
#34804=CARTESIAN_POINT('Ctrl Pts',(-4.94010734985006,-1.21630354408558,
-0.000802320355120511));
#34805=CARTESIAN_POINT('Ctrl Pts',(-5.00489265014995,-1.21648875695904,
-0.000697868307776));
#34806=CARTESIAN_POINT('Ctrl Pts',(-5.00247752477575,-1.2167683873322,-0.0415273680999158));
#34807=CARTESIAN_POINT('Ctrl Pts',(-5.00006239940156,-1.21489108992725,
-0.0823308472073769));
#34808=CARTESIAN_POINT('Ctrl Pts',(-4.99764727402736,-1.21077218381049,
-0.122906778219102));
#34809=CARTESIAN_POINT('Ctrl Pts',(-4.97382374645495,-1.17014204738398,
-0.523160041077697));
#34810=CARTESIAN_POINT('Ctrl Pts',(-4.95000021888253,-0.911393371578093,
-0.901271857920772));
#34811=CARTESIAN_POINT('Ctrl Pts',(-4.92617669131011,-0.553019227242496,
-1.08408721582794));
#34812=CARTESIAN_POINT('Ctrl Pts',(-4.9023531637377,-0.194645082906902,
-1.26690257373511));
#34813=CARTESIAN_POINT('Ctrl Pts',(-4.87852963616528,0.263354529958394,
-1.25442147270637));
#34814=CARTESIAN_POINT('Ctrl Pts',(-4.85470610859287,0.611240255558246,
-1.05235959025731));
#34815=CARTESIAN_POINT('Ctrl Pts',(-4.83088258102045,0.959125981158095,
-0.850297707808241));
#34816=CARTESIAN_POINT('Ctrl Pts',(-4.80705905344803,1.1968978194925,-0.458655043938839));
#34817=CARTESIAN_POINT('Ctrl Pts',(-4.78323552587562,1.21566897066551,-0.0567830166731548));
#34818=CARTESIAN_POINT('Ctrl Pts',(-4.7594119983032,1.23444012183852,0.345089010592532));
#34819=CARTESIAN_POINT('Ctrl Pts',(-4.73558847073079,1.03421058585014,0.757190401254506));
#34820=CARTESIAN_POINT('Ctrl Pts',(-4.71176494315838,0.706674793677344,
0.990800733347795));
#34821=CARTESIAN_POINT('Ctrl Pts',(-4.68794141558596,0.379139001504556,
1.22441106544108));
#34822=CARTESIAN_POINT('Ctrl Pts',(-4.66411788801354,-0.0757030468526306,
1.27953033896569));
#34823=CARTESIAN_POINT('Ctrl Pts',(-4.64029436044113,-0.449557991462852,
1.13091687118609));
#34824=CARTESIAN_POINT('Ctrl Pts',(-4.61647083286871,-0.823412936073079,
0.982303403406478));
#34825=CARTESIAN_POINT('Ctrl Pts',(-4.59264730529629,-1.11628077693633,
0.62995719432264));
#34826=CARTESIAN_POINT('Ctrl Pts',(-4.56882377772388,-1.19404368829401,
0.235233984931332));
#34827=CARTESIAN_POINT('Ctrl Pts',(-4.56418006853257,-1.20920132374984,
0.158294086341503));
#34828=CARTESIAN_POINT('Ctrl Pts',(-4.55953635934126,-1.21618620842765,
0.0797441053466365));
#34829=CARTESIAN_POINT('Ctrl Pts',(-4.55489265014995,-1.21546413760631,
0.00106646674887225));
#34830=CARTESIAN_POINT('Origin',(-3.875,0.,0.));
#34831=CARTESIAN_POINT('',(-4.04010734985006,-1.21302894219882,0.000187577549479595));
#34832=CARTESIAN_POINT('',(-4.10489265014995,-1.21300507934972,5.85455518045706E-5));
#34833=CARTESIAN_POINT('',(-3.875,-1.215,-1.48794586096403E-16));
#34834=CARTESIAN_POINT('Ctrl Pts',(-4.04010734985006,-1.21302894219882,
0.000187577549479595));
#34835=CARTESIAN_POINT('Ctrl Pts',(-4.05134597152774,-1.21329263069357,
0.191571241354318));
#34836=CARTESIAN_POINT('Ctrl Pts',(-4.06258459320541,-1.17069438186556,
0.382843920803326));
#34837=CARTESIAN_POINT('Ctrl Pts',(-4.07382321488309,-1.08461318382743,
0.551987029696823));
#34838=CARTESIAN_POINT('Ctrl Pts',(-4.09764674245551,-0.902139046540549,
0.910535046880482));
#34839=CARTESIAN_POINT('Ctrl Pts',(-4.12147027002792,-0.524273698081696,
1.16964354415799));
#34840=CARTESIAN_POINT('Ctrl Pts',(-4.14529379760034,-0.124059282017878,
1.21065467166778));
#34841=CARTESIAN_POINT('Ctrl Pts',(-4.16911732517275,0.276155134045952,
1.25166579917756));
#34842=CARTESIAN_POINT('Ctrl Pts',(-4.19294085274517,0.698718617714743,
1.07457955691961));
#34843=CARTESIAN_POINT('Ctrl Pts',(-4.21676438031759,0.950119667324172,
0.760491983685306));
#34844=CARTESIAN_POINT('Ctrl Pts',(-4.24058790789,1.20152071693359,0.446404410451012));
#34845=CARTESIAN_POINT('Ctrl Pts',(-4.26441143546242,1.28175933248366,-0.00468449375963097));
#34846=CARTESIAN_POINT('Ctrl Pts',(-4.28823496303483,1.154090514497,-0.386200108536821));
#34847=CARTESIAN_POINT('Ctrl Pts',(-4.31205849060725,1.02642169651034,-0.767715723314017));
#34848=CARTESIAN_POINT('Ctrl Pts',(-4.33588201817967,0.690845444986967,
-1.07965804865777));
#34849=CARTESIAN_POINT('Ctrl Pts',(-4.35970554575208,0.301037756232491,
-1.1791741638996));
#34850=CARTESIAN_POINT('Ctrl Pts',(-4.3835290733245,-0.0887699325219851,
-1.27869027914143));
#34851=CARTESIAN_POINT('Ctrl Pts',(-4.40735260089691,-0.532809058507552,
-1.16578018428134));
#34852=CARTESIAN_POINT('Ctrl Pts',(-4.43117612846932,-0.827733423133778,
-0.892150670970461));
#34853=CARTESIAN_POINT('Ctrl Pts',(-4.45081986892957,-1.07091393687214,
-0.666528872292524));
#34854=CARTESIAN_POINT('Ctrl Pts',(-4.47046360938981,-1.21271337931513,
-0.331636155886707));
#34855=CARTESIAN_POINT('Ctrl Pts',(-4.49010734985006,-1.21569869268569,
0.00101898845098317));
#34856=CARTESIAN_POINT('Ctrl Pts',(-4.55489265014995,-1.21546413760631,
0.00106646674887225));
#34857=CARTESIAN_POINT('Ctrl Pts',(-4.53571283176884,-1.21248178306146,
-0.323894196546626));
#34858=CARTESIAN_POINT('Ctrl Pts',(-4.51653301338774,-1.07802484522109,
-0.651032597879852));
#34859=CARTESIAN_POINT('Ctrl Pts',(-4.49735319500663,-0.844912941184178,
-0.87589809854854));
#34860=CARTESIAN_POINT('Ctrl Pts',(-4.47352966743422,-0.555361300864557,
-1.15520676293833));
#34861=CARTESIAN_POINT('Ctrl Pts',(-4.4497061398618,-0.113600038373203,
-1.27672388201915));
#34862=CARTESIAN_POINT('Ctrl Pts',(-4.42588261228938,0.278067787493538,
-1.18480110684447));
#34863=CARTESIAN_POINT('Ctrl Pts',(-4.40205908471697,0.669735613360282,
-1.0928783316698));
#34864=CARTESIAN_POINT('Ctrl Pts',(-4.37823555714455,1.01131000260242,-0.787515662239641));
#34865=CARTESIAN_POINT('Ctrl Pts',(-4.35441202957214,1.14636813226695,-0.408552888307276));
#34866=CARTESIAN_POINT('Ctrl Pts',(-4.33058850199972,1.28142626193149,-0.0295901143749137));
#34867=CARTESIAN_POINT('Ctrl Pts',(-4.3067649744273,1.20996813201843,0.422972764059648));
#34868=CARTESIAN_POINT('Ctrl Pts',(-4.28294144685489,0.964717748647626,
0.741886125133569));
#34869=CARTESIAN_POINT('Ctrl Pts',(-4.25911791928247,0.719467365276819,
1.06079948620749));
#34870=CARTESIAN_POINT('Ctrl Pts',(-4.23529439171006,0.300424728448258,
1.24606332992077));
#34871=CARTESIAN_POINT('Ctrl Pts',(-4.21147086413764,-0.100511019938621,
1.2128367128729));
#34872=CARTESIAN_POINT('Ctrl Pts',(-4.18764733656523,-0.501446768325502,
1.17961009582503));
#34873=CARTESIAN_POINT('Ctrl Pts',(-4.16382380899281,-0.884275628270695,
0.927893018016035));
#34874=CARTESIAN_POINT('Ctrl Pts',(-4.14000028142039,-1.0736824331033,0.572958454049525));
#34875=CARTESIAN_POINT('Ctrl Pts',(-4.12829773766358,-1.16672245056733,
0.398608234377028));
#34876=CARTESIAN_POINT('Ctrl Pts',(-4.11659519390676,-1.21309068378989,
0.199352146337624));
#34877=CARTESIAN_POINT('Ctrl Pts',(-4.10489265014995,-1.21300507934972,
5.85455518045706E-5));
#34878=CARTESIAN_POINT('Origin',(-3.875,0.,0.));
#34879=CARTESIAN_POINT('',(-3.59010734985006,-1.21500971925273,-0.00111129482518957));
#34880=CARTESIAN_POINT('',(-3.65489265014995,-1.21524902215508,-0.00109519578050164));
#34881=CARTESIAN_POINT('',(-3.875,-1.215,-1.48794586096403E-16));
#34882=CARTESIAN_POINT('Ctrl Pts',(-3.59010734985006,-1.21500971925273,
-0.00111129482518957));
#34883=CARTESIAN_POINT('Ctrl Pts',(-3.60840480609324,-1.21215498276526,
0.309197329221224));
#34884=CARTESIAN_POINT('Ctrl Pts',(-3.62670226233643,-1.09101085463479,
0.62148703039356));
#34885=CARTESIAN_POINT('Ctrl Pts',(-3.64499971857961,-0.87670201402857,
0.844078798504059));
#34886=CARTESIAN_POINT('Ctrl Pts',(-3.66882324615202,-0.597669097904114,
1.13389619467622));
#34887=CARTESIAN_POINT('Ctrl Pts',(-3.69264677372444,-0.160699812471054,
1.27165423805471));
#34888=CARTESIAN_POINT('Ctrl Pts',(-3.71647030129685,0.234097252973719,
1.19426710397464));
#34889=CARTESIAN_POINT('Ctrl Pts',(-3.74029382886927,0.628894318418485,
1.11687996989456));
#34890=CARTESIAN_POINT('Ctrl Pts',(-3.76411735644169,0.981519163874969,
0.824347658355936));
#34891=CARTESIAN_POINT('Ctrl Pts',(-3.7879408840141,1.13048844777284,0.45063434061106));
#34892=CARTESIAN_POINT('Ctrl Pts',(-3.81176441158652,1.27945773167071,0.0769210228661713));
#34893=CARTESIAN_POINT('Ctrl Pts',(-3.83558793915893,1.22477145400996,-0.377973301084966));
#34894=CARTESIAN_POINT('Ctrl Pts',(-3.85941146673135,0.99147300855165,-0.705731331881578));
#34895=CARTESIAN_POINT('Ctrl Pts',(-3.88323499430376,0.758174563093346,
-1.03348936267818));
#34896=CARTESIAN_POINT('Ctrl Pts',(-3.90705852187618,0.34626394983749,-1.23411110032026));
#34897=CARTESIAN_POINT('Ctrl Pts',(-3.93088204944859,-0.0556257751113993,
-1.21572250642532));
#34898=CARTESIAN_POINT('Ctrl Pts',(-3.95470557702101,-0.457515500060289,
-1.19733391253038));
#34899=CARTESIAN_POINT('Ctrl Pts',(-3.97852910459343,-0.849384336702215,
-0.959934987098434));
#34900=CARTESIAN_POINT('Ctrl Pts',(-4.00235263216584,-1.05177729196572,
-0.612241755837557));
#34901=CARTESIAN_POINT('Ctrl Pts',(-4.01493753806058,-1.15869245337526,
-0.428570946283624));
#34902=CARTESIAN_POINT('Ctrl Pts',(-4.02752244395532,-1.21273366623107,
-0.214122100972612));
#34903=CARTESIAN_POINT('Ctrl Pts',(-4.04010734985006,-1.21302894219882,
0.000187577549479595));
#34904=CARTESIAN_POINT('Ctrl Pts',(-4.10489265014995,-1.21300507934972,
5.85455518045706E-5));
#34905=CARTESIAN_POINT('Ctrl Pts',(-4.09277166633435,-1.21291641400863,
-0.206361063712259));
#34906=CARTESIAN_POINT('Ctrl Pts',(-4.08065068251875,-1.16299248122336,
-0.412820916319921));
#34907=CARTESIAN_POINT('Ctrl Pts',(-4.06852969870315,-1.06347545239199,
-0.59168853240628));
#34908=CARTESIAN_POINT('Ctrl Pts',(-4.04470617113073,-0.867876917128068,
-0.943248904771545));
#34909=CARTESIAN_POINT('Ctrl Pts',(-4.02088264355831,-0.480695096880224,
-1.18821759937806));
#34910=CARTESIAN_POINT('Ctrl Pts',(-3.9970591159859,-0.0792385815975481,
-1.21441204062207));
#34911=CARTESIAN_POINT('Ctrl Pts',(-3.97323558841348,0.322217933685125,
-1.24060648186608));
#34912=CARTESIAN_POINT('Ctrl Pts',(-3.94941206084107,0.737949144002628,
-1.04802666974759));
#34913=CARTESIAN_POINT('Ctrl Pts',(-3.92558853326865,0.97757236389716,-0.724863870368748));
#34914=CARTESIAN_POINT('Ctrl Pts',(-3.90176500569624,1.21719558379169,-0.401701070989909));
#34915=CARTESIAN_POINT('Ctrl Pts',(-3.87794147812382,1.28071081326325,0.0520447156492849));
#34916=CARTESIAN_POINT('Ctrl Pts',(-3.85411795055141,1.13903147027479,0.428582158920665));
#34917=CARTESIAN_POINT('Ctrl Pts',(-3.83029442297899,0.997352127286321,
0.805119602192056));
#34918=CARTESIAN_POINT('Ctrl Pts',(-3.80647089540658,0.650478211837817,
1.10444870209563));
#34919=CARTESIAN_POINT('Ctrl Pts',(-3.78264736783416,0.257259446777643,
1.18949272140064));
#34920=CARTESIAN_POINT('Ctrl Pts',(-3.75882384026174,-0.135959318282526,
1.27453674070565));
#34921=CARTESIAN_POINT('Ctrl Pts',(-3.73500031268933,-0.575522932954362,
1.14529567941211));
#34922=CARTESIAN_POINT('Ctrl Pts',(-3.71117678511691,-0.860134743741845,
0.860955039377548));
#34923=CARTESIAN_POINT('Ctrl Pts',(-3.69241540679459,-1.0842707303607,0.637032603714567));
#34924=CARTESIAN_POINT('Ctrl Pts',(-3.67365402847227,-1.21230879822748,
0.316920602375664));
#34925=CARTESIAN_POINT('Ctrl Pts',(-3.65489265014995,-1.21524902215508,
-0.00109519578050164));
#34926=CARTESIAN_POINT('Origin',(-3.875,0.,0.));
#34927=CARTESIAN_POINT('',(-3.14010734985006,-1.21677568176215,0.000466761158960617));
#34928=CARTESIAN_POINT('',(-3.20489265014995,-1.21663669410215,0.000593093442031073));
#34929=CARTESIAN_POINT('',(-3.875,-1.215,-1.48794586096403E-16));
#34930=CARTESIAN_POINT('Ctrl Pts',(-3.14010734985006,-1.21677568176215,
0.000466761158960617));
#34931=CARTESIAN_POINT('Ctrl Pts',(-3.14164011308633,-1.21690273304476,
0.0263631226345996));
#34932=CARTESIAN_POINT('Ctrl Pts',(-3.1431728763226,-1.21614766855925,0.0522519381467224));
#34933=CARTESIAN_POINT('Ctrl Pts',(-3.14470563955888,-1.21448695277727,
0.0780825269799757));
#34934=CARTESIAN_POINT('Ctrl Pts',(-3.16852916713129,-1.18867467643506,
0.479563806487453));
#34935=CARTESIAN_POINT('Ctrl Pts',(-3.19235269470371,-0.94407465143364,
0.866978652223446));
#34936=CARTESIAN_POINT('Ctrl Pts',(-3.21617622227613,-0.592700622392402,
1.0629117610138));
#34937=CARTESIAN_POINT('Ctrl Pts',(-3.23999974984854,-0.241326593351153,
1.25884486980417));
#34938=CARTESIAN_POINT('Ctrl Pts',(-3.26382327742096,0.216821439729918,
1.26329624164888));
#34939=CARTESIAN_POINT('Ctrl Pts',(-3.28764680499337,0.571936152525624,
1.07422738604077));
#34940=CARTESIAN_POINT('Ctrl Pts',(-3.31147033256579,0.927050865321321,
0.885158530432671));
#34941=CARTESIAN_POINT('Ctrl Pts',(-3.3352938601382,1.17913225783166,0.502569447371758));
#34942=CARTESIAN_POINT('Ctrl Pts',(-3.35911738771062,1.21274051878192,0.101665498525122));
#34943=CARTESIAN_POINT('Ctrl Pts',(-3.38294091528303,1.24634877973219,-0.299238450321518));
#34944=CARTESIAN_POINT('Ctrl Pts',(-3.40676444285545,1.06148390912237,-0.718457264953887));
#34945=CARTESIAN_POINT('Ctrl Pts',(-3.43058797042787,0.74280414198523,-0.964011123450032));
#34946=CARTESIAN_POINT('Ctrl Pts',(-3.45441149800028,0.424124374848083,
-1.20956498194618));
#34947=CARTESIAN_POINT('Ctrl Pts',(-3.4782350255727,-0.0283702888163973,
-1.28145388430611));
#34948=CARTESIAN_POINT('Ctrl Pts',(-3.50205855314511,-0.407461465865948,
-1.14675655364169));
#34949=CARTESIAN_POINT('Ctrl Pts',(-3.52588208071753,-0.786552642915494,
-1.01205922297728));
#34950=CARTESIAN_POINT('Ctrl Pts',(-3.54970560828994,-1.09224033335011,
-0.670775659288539));
#34951=CARTESIAN_POINT('Ctrl Pts',(-3.57352913586236,-1.18453590515949,
-0.279195502961247));
#34952=CARTESIAN_POINT('Ctrl Pts',(-3.57905520719159,-1.20594465378586,
-0.188365130825994));
#34953=CARTESIAN_POINT('Ctrl Pts',(-3.58458127852083,-1.21587188704514,
-0.0948285617373963));
#34954=CARTESIAN_POINT('Ctrl Pts',(-3.59010734985006,-1.21500971925273,
-0.00111129482518957));
#34955=CARTESIAN_POINT('Ctrl Pts',(-3.65489265014995,-1.21524902215508,
-0.00109519578050164));
#34956=CARTESIAN_POINT('Ctrl Pts',(-3.64983050089985,-1.21604234618994,
-0.0869014412757421));
#34957=CARTESIAN_POINT('Ctrl Pts',(-3.64476835164976,-1.20772835783292,
-0.172555080006382));
#34958=CARTESIAN_POINT('Ctrl Pts',(-3.63970620239967,-1.1897374078851,-0.25612547218169));
#34959=CARTESIAN_POINT('Ctrl Pts',(-3.61588267482725,-1.10506825433774,
-0.649425124930798));
#34960=CARTESIAN_POINT('Ctrl Pts',(-3.59205914725483,-0.806069940339887,
-0.996584211653431));
#34961=CARTESIAN_POINT('Ctrl Pts',(-3.56823561968242,-0.429667720848445,
-1.13862241629187));
#34962=CARTESIAN_POINT('Ctrl Pts',(-3.54441209211,-0.0532655013570036,-1.28066062093032));
#34963=CARTESIAN_POINT('Ctrl Pts',(-3.52058856453759,0.400540623628025,
-1.21757794348457));
#34964=CARTESIAN_POINT('Ctrl Pts',(-3.49676503696517,0.723931691739427,
-0.978262880271319));
#34965=CARTESIAN_POINT('Ctrl Pts',(-3.47294150939276,1.04732275985083,-0.73894781705807));
#34966=CARTESIAN_POINT('Ctrl Pts',(-3.44911798182034,1.2402987710886,-0.323400368077314));
#34967=CARTESIAN_POINT('Ctrl Pts',(-3.42529445424792,1.21448702131941,0.0780809340886104));
#34968=CARTESIAN_POINT('Ctrl Pts',(-3.40147092667551,1.18867527155022,0.479562236254538));
#34969=CARTESIAN_POINT('Ctrl Pts',(-3.37764739910309,0.944075760774064,
0.866977391605637));
#34970=CARTESIAN_POINT('Ctrl Pts',(-3.35382387153068,0.592701998122636,
1.06291095518057));
#34971=CARTESIAN_POINT('Ctrl Pts',(-3.33000034395826,0.241328235471213,
1.25884451875551));
#34972=CARTESIAN_POINT('Ctrl Pts',(-3.30617681638584,-0.216819779055476,
1.26329649055428));
#34973=CARTESIAN_POINT('Ctrl Pts',(-3.28235328881343,-0.57193472962917,
1.07422810532282));
#34974=CARTESIAN_POINT('Ctrl Pts',(-3.25852976124101,-0.927049680202874,
0.885159720091348));
#34975=CARTESIAN_POINT('Ctrl Pts',(-3.2347062336686,-1.17913156682357,0.502570977829626));
#34976=CARTESIAN_POINT('Ctrl Pts',(-3.21088270609618,-1.21274035194041,
0.101667084136921));
#34977=CARTESIAN_POINT('Ctrl Pts',(-3.20888602078077,-1.21555715425936,
0.0680667319223174));
#34978=CARTESIAN_POINT('Ctrl Pts',(-3.20688933546536,-1.2168393216259,0.0343377273868962));
#34979=CARTESIAN_POINT('Ctrl Pts',(-3.20489265014995,-1.21663669410215,
0.000593093442031074));
#34980=CARTESIAN_POINT('Origin',(-3.875,0.,0.));
#34981=CARTESIAN_POINT('',(-2.69010734985006,-1.21361800699981,0.000827517035146899));
#34982=CARTESIAN_POINT('',(-2.75489265014995,-1.21346326955177,0.000734265906742561));
#34983=CARTESIAN_POINT('',(-3.875,-1.215,-1.48794586096403E-16));
#34984=CARTESIAN_POINT('Ctrl Pts',(-2.69010734985006,-1.21361800699981,
0.000827517035146899));
#34985=CARTESIAN_POINT('Ctrl Pts',(-2.69869894765184,-1.21453325658579,
0.146957062172633));
#34986=CARTESIAN_POINT('Ctrl Pts',(-2.70729054545362,-1.19012564930912,
0.292791146029));
#34987=CARTESIAN_POINT('Ctrl Pts',(-2.71588214325539,-1.13903094055414,
0.428583662714895));
#34988=CARTESIAN_POINT('Ctrl Pts',(-2.73970567082781,-0.997351100446097,
0.805120930872916));
#34989=CARTESIAN_POINT('Ctrl Pts',(-2.76352919840022,-0.650476783306341,
1.10444958475712));
#34990=CARTESIAN_POINT('Ctrl Pts',(-2.78735272597264,-0.257257895936303,
1.18949309138987));
#34991=CARTESIAN_POINT('Ctrl Pts',(-2.81117625354506,0.135960991433729,
1.27453659802261));
#34992=CARTESIAN_POINT('Ctrl Pts',(-2.83499978111747,0.575524449034037,
1.1452949574039));
#34993=CARTESIAN_POINT('Ctrl Pts',(-2.85882330868989,0.860135895298941,
0.860953936691222));
#34994=CARTESIAN_POINT('Ctrl Pts',(-2.8826468362623,1.14474734156385,0.576612915978538));
#34995=CARTESIAN_POINT('Ctrl Pts',(-2.90647036383472,1.27440677649335,0.137172515171866));
#34996=CARTESIAN_POINT('Ctrl Pts',(-2.93029389140714,1.18973710545467,-0.256127037600748));
#34997=CARTESIAN_POINT('Ctrl Pts',(-2.95411741897955,1.105067434416,-0.649426590373356));
#34998=CARTESIAN_POINT('Ctrl Pts',(-2.97794094655197,0.806068657409177,
-0.996585295111915));
#34999=CARTESIAN_POINT('Ctrl Pts',(-3.00176447412438,0.429666241424461,
-1.13862301068702));
#35000=CARTESIAN_POINT('Ctrl Pts',(-3.0255880016968,0.0532638254397441,
-1.28066072626213));
#35001=CARTESIAN_POINT('Ctrl Pts',(-3.04941152926921,-0.400542229522857,
-1.21757745267379));
#35002=CARTESIAN_POINT('Ctrl Pts',(-3.07323505684163,-0.723932993162663,
-0.97826195924014));
#35003=CARTESIAN_POINT('Ctrl Pts',(-3.09552582117777,-1.0265173723596,-0.754343597448325));
#35004=CARTESIAN_POINT('Ctrl Pts',(-3.11781658551391,-1.21492799248291,
-0.376140451981686));
#35005=CARTESIAN_POINT('Ctrl Pts',(-3.14010734985006,-1.21677568176215,
0.000466761158960617));
#35006=CARTESIAN_POINT('Ctrl Pts',(-3.20489265014995,-1.21663669410215,
0.000593093442031074));
#35007=CARTESIAN_POINT('Ctrl Pts',(-3.18306580789294,-1.21442166353939,
-0.368287669315083));
#35008=CARTESIAN_POINT('Ctrl Pts',(-3.16123896563594,-1.03477582261886,
-0.739036123563579));
#35009=CARTESIAN_POINT('Ctrl Pts',(-3.13941212337893,-0.742805384007626,
-0.96401012375946));
#35010=CARTESIAN_POINT('Ctrl Pts',(-3.11558859580652,-0.424125947345048,
-1.20956439283947));
#35011=CARTESIAN_POINT('Ctrl Pts',(-3.0917650682341,0.0283686095930635,
-1.2814538858758));
#35012=CARTESIAN_POINT('Ctrl Pts',(-3.06794154066169,0.40745995253944,-1.14675705548211));
#35013=CARTESIAN_POINT('Ctrl Pts',(-3.04411801308927,0.786551295485811,
-1.01206022508842));
#35014=CARTESIAN_POINT('Ctrl Pts',(-3.02029448551685,1.09223942444044,-0.670777071264702));
#35015=CARTESIAN_POINT('Ctrl Pts',(-2.99647095794444,1.18453550657428,-0.279197046700459));
#35016=CARTESIAN_POINT('Ctrl Pts',(-2.97264743037202,1.27683158870812,0.112382977863789));
#35017=CARTESIAN_POINT('Ctrl Pts',(-2.94882390279961,1.15573562402117,0.55425987316857));
#35018=CARTESIAN_POINT('Ctrl Pts',(-2.92500037522719,0.876703095246122,
0.844077626766233));
#35019=CARTESIAN_POINT('Ctrl Pts',(-2.90117684765478,0.59767056647107,1.1338953803639));
#35020=CARTESIAN_POINT('Ctrl Pts',(-2.87735332008236,0.160701473607927,
1.27165399225445));
#35021=CARTESIAN_POINT('Ctrl Pts',(-2.85352979250994,-0.234095682233161,
1.19426737742485));
#35022=CARTESIAN_POINT('Ctrl Pts',(-2.82970626493753,-0.628892838074238,
1.11688076259526));
#35023=CARTESIAN_POINT('Ctrl Pts',(-2.80588273736512,-0.981518056893257,
0.82434892104552));
#35024=CARTESIAN_POINT('Ctrl Pts',(-2.7820592097927,-1.1304878261398,0.450635808798139));
#35025=CARTESIAN_POINT('Ctrl Pts',(-2.77300368991178,-1.18711246759842,
0.308584363753787));
#35026=CARTESIAN_POINT('Ctrl Pts',(-2.76394817003087,-1.21431250172664,
0.154803662174065));
#35027=CARTESIAN_POINT('Ctrl Pts',(-2.75489265014995,-1.21346326955177,
0.000734265906742561));
#35028=CARTESIAN_POINT('Origin',(-3.875,0.,0.));
#35029=CARTESIAN_POINT('',(-2.24010734985006,-1.21377365198237,-0.000902035925798433));
#35030=CARTESIAN_POINT('',(-2.30489265014994,-1.21396226950007,-0.000972860349384481));
#35031=CARTESIAN_POINT('',(-3.875,-1.215,-1.48794586096403E-16));
#35032=CARTESIAN_POINT('Ctrl Pts',(-2.24010734985006,-1.21377365198237,
-0.000902035925798433));
#35033=CARTESIAN_POINT('Ctrl Pts',(-2.25575778221734,-1.21194130236611,
0.265201375550419));
#35034=CARTESIAN_POINT('Ctrl Pts',(-2.27140821458463,-1.12582985342833,
0.532383292654391));
#35035=CARTESIAN_POINT('Ctrl Pts',(-2.28705864695191,-0.9647168037228,0.741887409314856));
#35036=CARTESIAN_POINT('Ctrl Pts',(-2.31088217452433,-0.719465995830789,
1.06080045801943));
#35037=CARTESIAN_POINT('Ctrl Pts',(-2.33470570209674,-0.300423104710086,
1.24606375801843));
#35038=CARTESIAN_POINT('Ctrl Pts',(-2.35852922966916,0.100512611290855,
1.21283661490585));
#35039=CARTESIAN_POINT('Ctrl Pts',(-2.38235275724157,0.501448327291784,
1.17960947179328));
#35040=CARTESIAN_POINT('Ctrl Pts',(-2.40617628481399,0.884276868172959,
0.927891885569145));
#35041=CARTESIAN_POINT('Ctrl Pts',(-2.4299998123864,1.07368321337605,0.572957063662786));
#35042=CARTESIAN_POINT('Ctrl Pts',(-2.45382333995882,1.26308955857914,0.218022241756422));
#35043=CARTESIAN_POINT('Ctrl Pts',(-2.47764686753124,1.25907370810414,-0.24012981583216));
#35044=CARTESIAN_POINT('Ctrl Pts',(-2.50147039510365,1.06347470693787,-0.591689941767681));
#35045=CARTESIAN_POINT('Ctrl Pts',(-2.52529392267607,0.867875705771602,
-0.943250067703207));
#35046=CARTESIAN_POINT('Ctrl Pts',(-2.54911745024848,0.480693553914047,
-1.18821826198566));
#35047=CARTESIAN_POINT('Ctrl Pts',(-2.5729409778209,0.0792369931733729,
-1.21441217813333));
#35048=CARTESIAN_POINT('Ctrl Pts',(-2.59676450539331,-0.32221956756729,
-1.24060609428099));
#35049=CARTESIAN_POINT('Ctrl Pts',(-2.62058803296573,-0.737950537191079,
-1.04802573229389));
#35050=CARTESIAN_POINT('Ctrl Pts',(-2.64441156053814,-0.977573340464803,
-0.724862610084428));
#35051=CARTESIAN_POINT('Ctrl Pts',(-2.65964349030878,-1.13077977472665,
-0.518243419580755));
#35052=CARTESIAN_POINT('Ctrl Pts',(-2.67487542007942,-1.21199537315011,
-0.258243615052597));
#35053=CARTESIAN_POINT('Ctrl Pts',(-2.69010734985006,-1.21361800699981,
0.000827517035146899));
#35054=CARTESIAN_POINT('Ctrl Pts',(-2.75489265014995,-1.21346326955177,
0.000734265906742561));
#35055=CARTESIAN_POINT('Ctrl Pts',(-2.74012464245845,-1.21207831678756,
-0.250526628997279));
#35056=CARTESIAN_POINT('Ctrl Pts',(-2.72535663476695,-1.13609341191021,
-0.502555337563078));
#35057=CARTESIAN_POINT('Ctrl Pts',(-2.71058862707545,-0.991473905375597,
-0.705730013660128));
#35058=CARTESIAN_POINT('Ctrl Pts',(-2.68676509950303,-0.758175895690786,
-1.03348834092597));
#35059=CARTESIAN_POINT('Ctrl Pts',(-2.66294157193062,-0.346265556647109,
-1.23411061251262));
#35060=CARTESIAN_POINT('Ctrl Pts',(-2.63911804435821,0.0556241812254146,
-1.21572254551951));
#35061=CARTESIAN_POINT('Ctrl Pts',(-2.61529451678579,0.457513919097938,
-1.1973344785264));
#35062=CARTESIAN_POINT('Ctrl Pts',(-2.59147098921337,0.849383055799309,
-0.959936072953527));
#35063=CARTESIAN_POINT('Ctrl Pts',(-2.56764746164095,1.05177646084693,-0.612243116441262));
#35064=CARTESIAN_POINT('Ctrl Pts',(-2.54382393406854,1.25416986589456,-0.264550159929002));
#35065=CARTESIAN_POINT('Ctrl Pts',(-2.52000040649613,1.26708753928845,0.193437347522645));
#35066=CARTESIAN_POINT('Ctrl Pts',(-2.49617687892371,1.08461387669191,0.551985593751234));
#35067=CARTESIAN_POINT('Ctrl Pts',(-2.4723533513513,0.902140214095379,0.910533839979817));
#35068=CARTESIAN_POINT('Ctrl Pts',(-2.44852982377888,0.524275215508423,
1.16964282498534));
#35069=CARTESIAN_POINT('Ctrl Pts',(-2.42470629620646,0.124060864275674,
1.21065447555299));
#35070=CARTESIAN_POINT('Ctrl Pts',(-2.40088276863405,-0.276153486957087,
1.25166612612065));
#35071=CARTESIAN_POINT('Ctrl Pts',(-2.37705924106163,-0.69871719083565,
1.07458044225042));
#35072=CARTESIAN_POINT('Ctrl Pts',(-2.35323571348922,-0.950118644851876,
0.760493207021673));
#35073=CARTESIAN_POINT('Ctrl Pts',(-2.33712135904279,-1.12016785885049,
0.548043013817145));
#35074=CARTESIAN_POINT('Ctrl Pts',(-2.32100700459637,-1.21190627045042,
0.272911350689318));
#35075=CARTESIAN_POINT('Ctrl Pts',(-2.30489265014994,-1.21396226950007,
-0.000972860349384481));
#35076=CARTESIAN_POINT('Origin',(-3.875,0.,0.));
#35077=CARTESIAN_POINT('',(-1.79010734985006,-1.21687501168408,-0.000345202031853675));
#35078=CARTESIAN_POINT('',(-1.85489265014995,-1.21695226826403,-0.000204119252572796));
#35079=CARTESIAN_POINT('',(-3.875,-1.215,-1.48794586096403E-16));
#35080=CARTESIAN_POINT('Ctrl Pts',(-1.79010734985006,-1.21687501168408,
-0.000345202031853675));
#35081=CARTESIAN_POINT('Ctrl Pts',(-1.81281661678285,-1.21543111614067,
0.383249301044499));
#35082=CARTESIAN_POINT('Ctrl Pts',(-1.83552588371564,-1.01889028811385,
0.768118048257717));
#35083=CARTESIAN_POINT('Ctrl Pts',(-1.85823515064843,-0.706673515517428,
0.990801686492171));
#35084=CARTESIAN_POINT('Ctrl Pts',(-1.88205867822084,-0.379137408229808,
1.22441159609891));
#35085=CARTESIAN_POINT('Ctrl Pts',(-1.90588220579326,0.0757047248680525,
1.27953027534214));
#35086=CARTESIAN_POINT('Ctrl Pts',(-1.92970573336567,0.449559485187943,
1.13091631374865));
#35087=CARTESIAN_POINT('Ctrl Pts',(-1.95352926093809,0.823414245507845,
0.982302352155159));
#35088=CARTESIAN_POINT('Ctrl Pts',(-1.97735278851051,1.11628163304977,0.629955749724934));
#35089=CARTESIAN_POINT('Ctrl Pts',(-2.00117631608292,1.19404402957313,0.235232427526729));
#35090=CARTESIAN_POINT('Ctrl Pts',(-2.02499984365534,1.27180642609648,-0.159490894671465));
#35091=CARTESIAN_POINT('Ctrl Pts',(-2.04882337122775,1.13446383160127,-0.596590936637636));
#35092=CARTESIAN_POINT('Ctrl Pts',(-2.07264689880017,0.844911817399206,
-0.87589922953649));
#35093=CARTESIAN_POINT('Ctrl Pts',(-2.09647042637258,0.555359803197147,
-1.15520752243534));
#35094=CARTESIAN_POINT('Ctrl Pts',(-2.120293953945,0.11359836928824,-1.27672406626688));
#35095=CARTESIAN_POINT('Ctrl Pts',(-2.14411748151742,-0.27806934705301,
-1.18480077553459));
#35096=CARTESIAN_POINT('Ctrl Pts',(-2.16794100908983,-0.669737063394275,
-1.09287748480229));
#35097=CARTESIAN_POINT('Ctrl Pts',(-2.19176453666225,-1.01131106216788,
-0.787514359506141));
#35098=CARTESIAN_POINT('Ctrl Pts',(-2.21558806423466,-1.14636869922301,
-0.408551398152983));
#35099=CARTESIAN_POINT('Ctrl Pts',(-2.2237611594398,-1.19270268240313,-0.278541249448389));
#35100=CARTESIAN_POINT('Ctrl Pts',(-2.23193425464493,-1.21473055639954,
-0.139868708881864));
#35101=CARTESIAN_POINT('Ctrl Pts',(-2.24010734985006,-1.21377365198237,
-0.000902035925798433));
#35102=CARTESIAN_POINT('Ctrl Pts',(-2.30489265014994,-1.21396226950007,
-0.000972860349384481));
#35103=CARTESIAN_POINT('Ctrl Pts',(-2.29718347702395,-1.21494586786098,
-0.13200018796546));
#35104=CARTESIAN_POINT('Ctrl Pts',(-2.28947430389796,-1.19540380974007,
-0.262742010627656));
#35105=CARTESIAN_POINT('Ctrl Pts',(-2.28176513077197,-1.15409098828612,
-0.386198586194984));
#35106=CARTESIAN_POINT('Ctrl Pts',(-2.25794160319955,-1.02642267355024,
-0.767714357595668));
#35107=CARTESIAN_POINT('Ctrl Pts',(-2.23411807562714,-0.690846839924569,
-1.07965711380979));
#35108=CARTESIAN_POINT('Ctrl Pts',(-2.21029454805472,-0.301039292341793,
-1.17917373685424));
#35109=CARTESIAN_POINT('Ctrl Pts',(-2.18647102048231,0.0887682552409884,
-1.27869035989869));
#35110=CARTESIAN_POINT('Ctrl Pts',(-2.16264749290989,0.532807516780883,
-1.16578084977346));
#35111=CARTESIAN_POINT('Ctrl Pts',(-2.13882396533747,0.827732231614367,
-0.892151730350494));
#35112=CARTESIAN_POINT('Ctrl Pts',(-2.11500043776506,1.12265694644784,-0.618522610927539));
#35113=CARTESIAN_POINT('Ctrl Pts',(-2.09117691019264,1.26846711457492,-0.184173882206858));
#35114=CARTESIAN_POINT('Ctrl Pts',(-2.06735338262023,1.1983894683434,0.211985941492073));
#35115=CARTESIAN_POINT('Ctrl Pts',(-2.04352985504781,1.12831182211188,0.608145765191016));
#35116=CARTESIAN_POINT('Ctrl Pts',(-2.01970632747539,0.842346361521747,
0.966116683868196));
#35117=CARTESIAN_POINT('Ctrl Pts',(-1.99588279990298,0.471449990912945,
1.12196714001866));
#35118=CARTESIAN_POINT('Ctrl Pts',(-1.97205927233056,0.100553620304143,
1.27781759616912));
#35119=CARTESIAN_POINT('Ctrl Pts',(-1.94823574475815,-0.355273660323328,
1.23154758979285));
#35120=CARTESIAN_POINT('Ctrl Pts',(-1.92441221718573,-0.687287307315033,
1.00434631199737));
#35121=CARTESIAN_POINT('Ctrl Pts',(-1.9012390281738,-1.01023759135217,0.783347211922782));
#35122=CARTESIAN_POINT('Ctrl Pts',(-1.87806583916187,-1.21604174683208,
0.391160195305395));
#35123=CARTESIAN_POINT('Ctrl Pts',(-1.85489265014995,-1.21695226826403,
-0.000204119252572796));
#35124=CARTESIAN_POINT('Origin',(-3.875,0.,0.));
#35125=CARTESIAN_POINT('',(-1.34010734985006,-1.2147956596487,0.00111167046010718));
#35126=CARTESIAN_POINT('',(-1.40489265014995,-1.21456320713733,0.00109666547093623));
#35127=CARTESIAN_POINT('',(-3.875,-1.215,-1.48794586096403E-16));
#35128=CARTESIAN_POINT('Ctrl Pts',(-1.34010734985006,-1.2147956596487,0.00111167046010718));
#35129=CARTESIAN_POINT('Ctrl Pts',(-1.34605192377594,-1.2157089644333,0.101971735915578));
#35130=CARTESIAN_POINT('Ctrl Pts',(-1.35199649770182,-1.20419912218747,
0.202626225854525));
#35131=CARTESIAN_POINT('Ctrl Pts',(-1.3579410716277,-1.17945980404156,0.299916684419064));
#35132=CARTESIAN_POINT('Ctrl Pts',(-1.38176459920011,-1.08031429162624,
0.689818795326428));
#35133=CARTESIAN_POINT('Ctrl Pts',(-1.40558812677253,-0.768691101236954,
1.02569143594608));
#35134=CARTESIAN_POINT('Ctrl Pts',(-1.42941165434494,-0.387297020092423,
1.15372286954436));
#35135=CARTESIAN_POINT('Ctrl Pts',(-1.45323518191736,-0.00590293894791455,
1.28175430314263));
#35136=CARTESIAN_POINT('Ctrl Pts',(-1.47705870948977,0.44526203295183,1.20194452971952));
#35137=CARTESIAN_POINT('Ctrl Pts',(-1.50088223706219,0.759588447271108,
0.950842167264673));
#35138=CARTESIAN_POINT('Ctrl Pts',(-1.52470576463461,1.07391486159039,0.699739804809822));
#35139=CARTESIAN_POINT('Ctrl Pts',(-1.54852929220702,1.25140271832922,0.277344853323226));
#35140=CARTESIAN_POINT('Ctrl Pts',(-1.57235281977944,1.21077205702477,-0.122908367057554));
#35141=CARTESIAN_POINT('Ctrl Pts',(-1.59617634735185,1.17014139572032,-0.523161587438345));
#35142=CARTESIAN_POINT('Ctrl Pts',(-1.61999987492427,0.911392216372567,
-0.90127307671332));
#35143=CARTESIAN_POINT('Ctrl Pts',(-1.64382340249668,0.553017822372426,
-1.0840879705008));
#35144=CARTESIAN_POINT('Ctrl Pts',(-1.6676469300691,0.194643428372295,-1.26690286428827));
#35145=CARTESIAN_POINT('Ctrl Pts',(-1.69147045764152,-0.263356180280222,
-1.25442116258826));
#35146=CARTESIAN_POINT('Ctrl Pts',(-1.71529398521393,-0.611241650744325,
-1.05235881876606));
#35147=CARTESIAN_POINT('Ctrl Pts',(-1.73911751278635,-0.959127121208428,
-0.85029647494387));
#35148=CARTESIAN_POINT('Ctrl Pts',(-1.76294104035876,-1.19689845348412,
-0.458653488999493));
#35149=CARTESIAN_POINT('Ctrl Pts',(-1.78676456793118,-1.21566907888328,
-0.0567814260421754));
#35150=CARTESIAN_POINT('Ctrl Pts',(-1.7878788285708,-1.21654700802286,-0.0379852918190725));
#35151=CARTESIAN_POINT('Ctrl Pts',(-1.78899308921043,-1.21694585835547,
-0.0191667808005626));
#35152=CARTESIAN_POINT('Ctrl Pts',(-1.79010734985006,-1.21687501168408,
-0.000345202031853675));
#35153=CARTESIAN_POINT('Ctrl Pts',(-1.85489265014995,-1.21695226826403,
-0.000204119252572796));
#35154=CARTESIAN_POINT('Ctrl Pts',(-1.85424231158946,-1.21697782138048,
-0.0111874718168012));
#35155=CARTESIAN_POINT('Ctrl Pts',(-1.85359197302897,-1.21684199964081,
-0.0221701764183581));
#35156=CARTESIAN_POINT('Ctrl Pts',(-1.85294163446849,-1.21654286351776,
-0.0331484310200425));
#35157=CARTESIAN_POINT('Ctrl Pts',(-1.82911810689607,-1.20558475937286,
-0.435309347027362));
#35158=CARTESIAN_POINT('Ctrl Pts',(-1.80529457932365,-0.975468537727084,
-0.831498629827334));
#35159=CARTESIAN_POINT('Ctrl Pts',(-1.78147105175124,-0.631575135093402,
-1.04028275285737));
#35160=CARTESIAN_POINT('Ctrl Pts',(-1.75764752417882,-0.287681732459729,
-1.24906687588741));
#35161=CARTESIAN_POINT('Ctrl Pts',(-1.7338239966064,0.169988851161846,-1.27044583914752));
#35162=CARTESIAN_POINT('Ctrl Pts',(-1.71000046903399,0.531847937959752,
-1.09462921946797));
#35163=CARTESIAN_POINT('Ctrl Pts',(-1.68617694146157,0.893707024757658,
-0.918812599788423));
#35164=CARTESIAN_POINT('Ctrl Pts',(-1.66235341388916,1.15975461473189,-0.545800397169212));
#35165=CARTESIAN_POINT('Ctrl Pts',(-1.63852988631674,1.20815512394341,-0.146412273808625));
#35166=CARTESIAN_POINT('Ctrl Pts',(-1.61470635874433,1.25655563315493,0.252975849551963));
#35167=CARTESIAN_POINT('Ctrl Pts',(-1.59088283117191,1.08730906160373,0.678739893653927));
#35168=CARTESIAN_POINT('Ctrl Pts',(-1.5670593035995,0.777921298304252,0.935902671445341));
#35169=CARTESIAN_POINT('Ctrl Pts',(-1.54323577602708,0.46853353500476,1.19306544923676));
#35170=CARTESIAN_POINT('Ctrl Pts',(-1.51941224845466,0.0190045799569751,
1.28162696071762));
#35171=CARTESIAN_POINT('Ctrl Pts',(-1.49558872088225,-0.364805320954119,
1.16103076409948));
#35172=CARTESIAN_POINT('Ctrl Pts',(-1.47176519330983,-0.748615221865207,
1.04043456748134));
#35173=CARTESIAN_POINT('Ctrl Pts',(-1.44794166573742,-1.06670606863961,
0.710680662764208));
#35174=CARTESIAN_POINT('Ctrl Pts',(-1.424118138165,-1.17340924408634,0.322778723580791));
#35175=CARTESIAN_POINT('Ctrl Pts',(-1.41770964215998,-1.20211225087217,
0.218433637823035));
#35176=CARTESIAN_POINT('Ctrl Pts',(-1.41130114615496,-1.21551919148474,
0.109880945361187));
#35177=CARTESIAN_POINT('Ctrl Pts',(-1.40489265014995,-1.21456320713733,
0.00109666547093623));
#35178=CARTESIAN_POINT('Origin',(-3.875,0.,0.));
#35179=CARTESIAN_POINT('',(-0.890107349850054,-1.21307144811218,-0.000301679661677823));
#35180=CARTESIAN_POINT('',(-0.954892650149944,-1.21314228096755,-0.000424764636864103));
#35181=CARTESIAN_POINT('',(-3.875,-1.215,-1.48794586096403E-16));
#35182=CARTESIAN_POINT('Ctrl Pts',(-0.890107349850054,-1.21307144811218,
-0.000301679661677823));
#35183=CARTESIAN_POINT('Ctrl Pts',(-0.903110758341441,-1.21257958185045,
0.221115114836065));
#35184=CARTESIAN_POINT('Ctrl Pts',(-0.916114166832826,-1.15466388054098,
0.442771501567673));
#35185=CARTESIAN_POINT('Ctrl Pts',(-0.929117575324213,-1.04088370137469,
0.630584464127237));
#35186=CARTESIAN_POINT('Ctrl Pts',(-0.952941102896628,-0.832427184965302,
0.974676345495014));
#35187=CARTESIAN_POINT('Ctrl Pts',(-0.976764630469044,-0.436456767496894,
1.20516987715727));
#35188=CARTESIAN_POINT('Ctrl Pts',(-1.00058815804146,-0.034306369757509,
1.21651086436758));
#35189=CARTESIAN_POINT('Ctrl Pts',(-1.02441168561388,0.367844027981887,
1.22785185157789));
#35190=CARTESIAN_POINT('Ctrl Pts',(-1.04823521318629,0.776174405992254,
1.02004029433626));
#35191=CARTESIAN_POINT('Ctrl Pts',(-1.07205874075871,1.00369159274397,0.688243032164823));
#35192=CARTESIAN_POINT('Ctrl Pts',(-1.09588226833112,1.23120877949568,0.356445769993402));
#35193=CARTESIAN_POINT('Ctrl Pts',(-1.11970579590354,1.27791277498875,-0.09933719710782));
#35194=CARTESIAN_POINT('Ctrl Pts',(-1.14352932347595,1.12241547143391,-0.470381749254917));
#35195=CARTESIAN_POINT('Ctrl Pts',(-1.16735285104837,0.966918167879057,
-0.84142630140202));
#35196=CARTESIAN_POINT('Ctrl Pts',(-1.19117637862078,0.60921956527629,-1.12773243859501));
#35197=CARTESIAN_POINT('Ctrl Pts',(-1.2149999061932,0.213126605972733,-1.1981871760399));
#35198=CARTESIAN_POINT('Ctrl Pts',(-1.23882343376562,-0.182966353330836,
-1.26864191348479));
#35199=CARTESIAN_POINT('Ctrl Pts',(-1.26264696133803,-0.61745366933519,
-1.12324525118158));
#35200=CARTESIAN_POINT('Ctrl Pts',(-1.28647048891045,-0.891363410116701,
-0.828581129432447));
#35201=CARTESIAN_POINT('Ctrl Pts',(-1.30434944255699,-1.09692572845437,
-0.607443174189));
#35202=CARTESIAN_POINT('Ctrl Pts',(-1.32222839620352,-1.21204879601934,
-0.302235963457676));
#35203=CARTESIAN_POINT('Ctrl Pts',(-1.34010734985006,-1.2147956596487,0.00111167046010718));
#35204=CARTESIAN_POINT('Ctrl Pts',(-1.40489265014995,-1.21456320713733,
0.00109666547093623));
#35205=CARTESIAN_POINT('Ctrl Pts',(-1.38747761858255,-1.21196532807569,
-0.294523658992334));
#35206=CARTESIAN_POINT('Ctrl Pts',(-1.37006258701515,-1.10330071711548,
-0.591854200681401));
#35207=CARTESIAN_POINT('Ctrl Pts',(-1.35264755544775,-0.907295667300257,
-0.811104140109695));
#35208=CARTESIAN_POINT('Ctrl Pts',(-1.32882402787534,-0.639163410948359,
-1.11103509096706));
#35209=CARTESIAN_POINT('Ctrl Pts',(-1.30500050030292,-0.207583394125489,
-1.2648470190321));
#35210=CARTESIAN_POINT('Ctrl Pts',(-1.28117697273051,0.189803798807097,
-1.20210227400952));
#35211=CARTESIAN_POINT('Ctrl Pts',(-1.25735344515809,0.587190991739688,
-1.13935752898695));
#35212=CARTESIAN_POINT('Ctrl Pts',(-1.23352991758568,0.950385360781995,
-0.860056110876766));
#35213=CARTESIAN_POINT('Ctrl Pts',(-1.20970639001326,1.11306327236761,-0.492103156261569));
#35214=CARTESIAN_POINT('Ctrl Pts',(-1.18588286244084,1.27574118395322,-0.124150201646372));
#35215=CARTESIAN_POINT('Ctrl Pts',(-1.16205933486843,1.23790263808214,0.332454289473836));
#35216=CARTESIAN_POINT('Ctrl Pts',(-1.13823580729601,1.01687569553182,0.668609867168432));
#35217=CARTESIAN_POINT('Ctrl Pts',(-1.1144122797236,0.795848752981512,1.00476544486302));
#35218=CARTESIAN_POINT('Ctrl Pts',(-1.09058875215118,0.391633413751968,
1.22047210913201));
#35219=CARTESIAN_POINT('Ctrl Pts',(-1.06676522457877,-0.0106613438959427,
1.21694770327565));
#35220=CARTESIAN_POINT('Ctrl Pts',(-1.04294169700635,-0.412956101543859,
1.21342329741929));
#35221=CARTESIAN_POINT('Ctrl Pts',(-1.01911816943393,-0.813330277610143,
0.990667821437577));
#35222=CARTESIAN_POINT('Ctrl Pts',(-0.995294641861518,-1.02843378651698,
0.650691436184902));
#35223=CARTESIAN_POINT('Ctrl Pts',(-0.981827311290994,-1.15003081082509,
0.458504349178061));
#35224=CARTESIAN_POINT('Ctrl Pts',(-0.968359980720469,-1.21242294632906,
0.228858278483662));
#35225=CARTESIAN_POINT('Ctrl Pts',(-0.954892650149944,-1.21314228096755,
-0.000424764636864103));
#35226=CARTESIAN_POINT('Origin',(-3.875,0.,0.));
#35227=CARTESIAN_POINT('',(-0.440107349850056,-1.21588398405722,-0.000947377684412109));
#35228=CARTESIAN_POINT('',(-0.504892650149942,-1.2161173910499,-0.000883162254970131));
#35229=CARTESIAN_POINT('',(-3.875,-1.215,-1.48794586096403E-16));
#35230=CARTESIAN_POINT('Ctrl Pts',(-0.440107349850056,-1.21588398405722,
-0.000947377684412109));
#35231=CARTESIAN_POINT('Ctrl Pts',(-0.460169592906947,-1.21293866576822,
0.338647307153245));
#35232=CARTESIAN_POINT('Ctrl Pts',(-0.480231835963839,-1.06433222539992,
0.680481871379908));
#35233=CARTESIAN_POINT('Ctrl Pts',(-0.50029407902073,-0.811976032752873,
0.906516706944358));
#35234=CARTESIAN_POINT('Ctrl Pts',(-0.524117606593145,-0.512307910073469,
1.17492872458993));
#35235=CARTESIAN_POINT('Ctrl Pts',(-0.547941134165561,-0.0663411673267536,
1.2800503233636));
#35236=CARTESIAN_POINT('Ctrl Pts',(-0.571764661737977,0.321666109547873,
1.17371941224906));
#35237=CARTESIAN_POINT('Ctrl Pts',(-0.595588189310392,0.709673386422499,
1.06738850113453));
#35238=CARTESIAN_POINT('Ctrl Pts',(-0.619411716882807,1.03972119742504,
0.749605080131778));
#35239=CARTESIAN_POINT('Ctrl Pts',(-0.643235244455223,1.16068062812135,
0.365908576638235));
#35240=CARTESIAN_POINT('Ctrl Pts',(-0.667058772027639,1.28164005881766,
-0.0177879268553193));
#35241=CARTESIAN_POINT('Ctrl Pts',(-0.690882299600056,1.19351110920773,
-0.467397512839677));
#35242=CARTESIAN_POINT('Ctrl Pts',(-0.714705827172472,0.936644043228513,
-0.777029118824175));
#35243=CARTESIAN_POINT('Ctrl Pts',(-0.738529354744887,0.679776977249306,
-1.08666072480866));
#35244=CARTESIAN_POINT('Ctrl Pts',(-0.762352882317302,0.254171794900829,
-1.2563143507933));
#35245=CARTESIAN_POINT('Ctrl Pts',(-0.786176409889718,-0.145262806446263,
-1.20829448088716));
#35246=CARTESIAN_POINT('Ctrl Pts',(-0.809999937462134,-0.54469740779336,
-1.16027461098102));
#35247=CARTESIAN_POINT('Ctrl Pts',(-0.83382346503455,-0.917961428139059,
-0.894581245184098));
#35248=CARTESIAN_POINT('Ctrl Pts',(-0.857646992606965,-1.09412213063674,
-0.532889446748983));
#35249=CARTESIAN_POINT('Ctrl Pts',(-0.868467111687995,-1.17413042380949,
-0.368617035041528));
#35250=CARTESIAN_POINT('Ctrl Pts',(-0.879287230769025,-1.21348072938081,
-0.184542302771571));
#35251=CARTESIAN_POINT('Ctrl Pts',(-0.890107349850054,-1.21307144811218,
-0.000301679661677823));
#35252=CARTESIAN_POINT('Ctrl Pts',(-0.954892650149944,-1.21314228096755,
-0.000424764636864103));
#35253=CARTESIAN_POINT('Ctrl Pts',(-0.944536453148053,-1.2136954396791,
-0.176740356751778));
#35254=CARTESIAN_POINT('Ctrl Pts',(-0.934180256146162,-1.17777897841535,
-0.352841275988632));
#35255=CARTESIAN_POINT('Ctrl Pts',(-0.92382405914427,-1.10427065644089,
-0.511528610604347));
#35256=CARTESIAN_POINT('Ctrl Pts',(-0.900000531571855,-0.935171175710573,
-0.876574977617282));
#35257=CARTESIAN_POINT('Ctrl Pts',(-0.87617700399944,-0.567139372502564,
-1.14947041711951));
#35258=CARTESIAN_POINT('Ctrl Pts',(-0.852353476427024,-0.168713786606679,
-1.20524320627726));
#35259=CARTESIAN_POINT('Ctrl Pts',(-0.828529948854608,0.2297117992892,-1.26101599543501));
#35260=CARTESIAN_POINT('Ctrl Pts',(-0.804706421282191,0.658531167872964,
-1.09966613424829));
#35261=CARTESIAN_POINT('Ctrl Pts',(-0.780882893709776,0.921367262878983,
-0.795083600172721));
#35262=CARTESIAN_POINT('Ctrl Pts',(-0.75705936613736,1.18420335788501,-0.49050106609715));
#35263=CARTESIAN_POINT('Ctrl Pts',(-0.733235838564946,1.28105617931329,
-0.0426858591327475));
#35264=CARTESIAN_POINT('Ctrl Pts',(-0.70941231099253,1.1675736252803,0.343287263096404));
#35265=CARTESIAN_POINT('Ctrl Pts',(-0.685588783420115,1.0540910712473,0.729260385325549));
#35266=CARTESIAN_POINT('Ctrl Pts',(-0.661765255847698,0.730273141753013,
1.05339142281944));
#35267=CARTESIAN_POINT('Ctrl Pts',(-0.637941728275282,0.344408651243341,
1.16724437696144));
#35268=CARTESIAN_POINT('Ctrl Pts',(-0.614118200702865,-0.0414558392663365,
1.28109733110344));
#35269=CARTESIAN_POINT('Ctrl Pts',(-0.59029467313045,-0.489366890791401,
1.18467220189356));
#35270=CARTESIAN_POINT('Ctrl Pts',(-0.566471145558034,-0.794200427296363,
0.922129012820161));
#35271=CARTESIAN_POINT('Ctrl Pts',(-0.545944980422003,-1.0568426195696,
0.695923853324785));
#35272=CARTESIAN_POINT('Ctrl Pts',(-0.525418815285973,-1.2132724933316,
0.346402432135793));
#35273=CARTESIAN_POINT('Ctrl Pts',(-0.504892650149942,-1.2161173910499,
-0.000883162254970131));
#35274=CARTESIAN_POINT('Origin',(-3.875,0.,0.));
#35275=CARTESIAN_POINT('',(1.11022302462516E-15,-1.215,-1.48794586096403E-16));
#35276=CARTESIAN_POINT('',(-0.0548926501499415,-1.2158567361346,0.000987498914498598));
#35277=CARTESIAN_POINT('',(-3.875,-1.215,-1.48794586096403E-16));
#35278=CARTESIAN_POINT('',(0.,-1.20342780657953,0.167291704370512));
#35279=CARTESIAN_POINT('Origin',(0.,0.,0.));
#35280=CARTESIAN_POINT('Ctrl Pts',(1.10154940724527E-15,-1.20342780657953,
0.167291704370495));
#35281=CARTESIAN_POINT('Ctrl Pts',(-0.0238235275724144,-1.14778002846286,
0.567598962951908));
#35282=CARTESIAN_POINT('Ctrl Pts',(-0.0476470551448301,-0.877196554917926,
0.934492539965354));
#35283=CARTESIAN_POINT('Ctrl Pts',(-0.0714705827172457,-0.512872496153858,
1.10355045672817));
#35284=CARTESIAN_POINT('Ctrl Pts',(-0.095294110289662,-0.148548437389779,
1.27260837349098));
#35285=CARTESIAN_POINT('Ctrl Pts',(-0.119117637862078,0.309516206593437,
1.24383063000316));
#35286=CARTESIAN_POINT('Ctrl Pts',(-0.142941165434494,0.649908400043695,
1.02920423803292));
#35287=CARTESIAN_POINT('Ctrl Pts',(-0.16676469300691,0.990300593493944,
0.814577846062692));
#35288=CARTESIAN_POINT('Ctrl Pts',(-0.190588220579325,1.21302033641124,
0.414102805610063));
#35289=CARTESIAN_POINT('Ctrl Pts',(-0.214411748151741,1.21682758227759,
0.0117367051186408));
#35290=CARTESIAN_POINT('Ctrl Pts',(-0.238235275724156,1.22063482814394,
-0.390629395372782));
#35291=CARTESIAN_POINT('Ctrl Pts',(-0.262058803296572,1.00552957695933,
-0.794886555902997));
#35292=CARTESIAN_POINT('Ctrl Pts',(-0.285882330868987,0.669635953571026,
-1.01619465631964));
#35293=CARTESIAN_POINT('Ctrl Pts',(-0.309705858441404,0.333742330182708,
-1.23750275673629));
#35294=CARTESIAN_POINT('Ctrl Pts',(-0.333529386013819,-0.122939665409323,
-1.27586179703936));
#35295=CARTESIAN_POINT('Ctrl Pts',(-0.357352913586235,-0.491074246481195,
-1.11355454158985));
#35296=CARTESIAN_POINT('Ctrl Pts',(-0.381176441158651,-0.859208827553056,
-0.951247286140343));
#35297=CARTESIAN_POINT('Ctrl Pts',(-0.404999968731066,-1.13879599410476,
-0.588273734938262));
#35298=CARTESIAN_POINT('Ctrl Pts',(-0.428823496303482,-1.20190482607457,
-0.190935741078487));
#35299=CARTESIAN_POINT('Ctrl Pts',(-0.432584780819007,-1.21186851729366,
-0.128203585263544));
#35300=CARTESIAN_POINT('Ctrl Pts',(-0.436346065334531,-1.21643617455966,
-0.0646148462726548));
#35301=CARTESIAN_POINT('Ctrl Pts',(-0.440107349850056,-1.21588398405722,
-0.000947377684412109));
#35302=CARTESIAN_POINT('Ctrl Pts',(-0.504892650149942,-1.2161173910499,
-0.000883162254970131));
#35303=CARTESIAN_POINT('Ctrl Pts',(-0.501595287713558,-1.21657440086199,
-0.0566717845354851));
#35304=CARTESIAN_POINT('Ctrl Pts',(-0.498297925277174,-1.21306802377492,
-0.112402709462593));
#35305=CARTESIAN_POINT('Ctrl Pts',(-0.495000562840789,-1.20540187658012,
-0.167555461232997));
#35306=CARTESIAN_POINT('Ctrl Pts',(-0.471177035268374,-1.15001376787406,
-0.566035497275865));
#35307=CARTESIAN_POINT('Ctrl Pts',(-0.447353507695957,-0.877481528977088,
-0.934334320424685));
#35308=CARTESIAN_POINT('Ctrl Pts',(-0.423529980123542,-0.512593280682101,
-1.10378186225489));
#35309=CARTESIAN_POINT('Ctrl Pts',(-0.399706452551125,-0.147705032387104,
-1.2732294040851));
#35310=CARTESIAN_POINT('Ctrl Pts',(-0.375882924978708,0.309539225305917,
-1.24382566459669));
#35311=CARTESIAN_POINT('Ctrl Pts',(-0.352059397406292,0.649713618299758,
-1.0290528454463));
#35312=CARTESIAN_POINT('Ctrl Pts',(-0.328235869833877,0.989888011293583,
-0.814280026295927));
#35313=CARTESIAN_POINT('Ctrl Pts',(-0.304412342261461,1.21299253958824,
-0.414138127483595));
#35314=CARTESIAN_POINT('Ctrl Pts',(-0.280588814689046,1.21691880955427,
-0.0118387594639543));
#35315=CARTESIAN_POINT('Ctrl Pts',(-0.25676528711663,1.22084507952029,0.390460608555698));
#35316=CARTESIAN_POINT('Ctrl Pts',(-0.232941759544215,1.00559309115768,
0.794917445782652));
#35317=CARTESIAN_POINT('Ctrl Pts',(-0.209118231971799,0.6696198577145,1.01625136658536));
#35318=CARTESIAN_POINT('Ctrl Pts',(-0.185294704399383,0.333646624271334,
1.23758528738806));
#35319=CARTESIAN_POINT('Ctrl Pts',(-0.161471176826967,-0.123047854252383,
1.27579629176651));
#35320=CARTESIAN_POINT('Ctrl Pts',(-0.137647649254552,-0.491099606844063,
1.11350124652694));
#35321=CARTESIAN_POINT('Ctrl Pts',(-0.113824121682136,-0.859151359435747,
0.95120620128737));
#35322=CARTESIAN_POINT('Ctrl Pts',(-0.0900005941097201,-1.1385603860954,
0.588405106429774));
#35323=CARTESIAN_POINT('Ctrl Pts',(-0.0661770665373044,-1.20179772134079,
0.191021162694664));
#35324=CARTESIAN_POINT('Ctrl Pts',(-0.0624155944081834,-1.21178219879999,
0.128278622809408));
#35325=CARTESIAN_POINT('Ctrl Pts',(-0.0586541222790624,-1.21637774826694,
0.0646739696606226));
#35326=CARTESIAN_POINT('Ctrl Pts',(-0.0548926501499415,-1.2158567361346,
0.000987498914498598));
#35327=CARTESIAN_POINT('Origin',(-8.61687266823562,0.,0.));
#35328=CARTESIAN_POINT('',(-0.291872668235618,-0.958947183310973,-0.000747180795175678));
#35329=CARTESIAN_POINT('',(-0.203127331764369,-0.958925693334137,0.000778823732210353));
#35330=CARTESIAN_POINT('',(-8.61687266823562,-0.95825,-1.32069628103871E-13));
#35331=CARTESIAN_POINT('',(-1.1100891904241E-15,0.570663296631698,0.771750790290221));
#35332=CARTESIAN_POINT('Ctrl Pts',(-0.291872668235618,-0.958947183310973,
-0.000747180795175641));
#35333=CARTESIAN_POINT('Ctrl Pts',(-0.288111383720094,-0.959382686643452,
-0.0509606390459395));
#35334=CARTESIAN_POINT('Ctrl Pts',(-0.260526571632154,-0.932962863692293,
-0.418764773197866));
#35335=CARTESIAN_POINT('Ctrl Pts',(-0.209118231971798,-0.457137824406994,
-1.03650380031556));
#35336=CARTESIAN_POINT('Ctrl Pts',(-0.137647649254552,0.62339432936104,
-0.945744416684868));
#35337=CARTESIAN_POINT('Ctrl Pts',(-0.0679415719306187,1.11977874493364,
-0.0128664266509041));
#35338=CARTESIAN_POINT('Ctrl Pts',(-0.0220590221791022,0.806106298516984,
0.59564865151797));
#35339=CARTESIAN_POINT('Ctrl Pts',(-1.14112278654099E-15,0.570663374910285,
0.771750967939217));
#35340=CARTESIAN_POINT('',(0.,0.913908649078052,-0.288121577880467));
#35341=CARTESIAN_POINT('Origin',(0.,0.,0.));
#35342=CARTESIAN_POINT('Ctrl Pts',(-0.203127331764369,-0.958925693334137,
0.000778823732210361));
#35343=CARTESIAN_POINT('Ctrl Pts',(-0.183065276321077,-0.956734059660944,
-0.267117843441326));
#35344=CARTESIAN_POINT('Ctrl Pts',(-0.13917969330537,-0.700830832226228,
-0.857155041760208));
#35345=CARTESIAN_POINT('Ctrl Pts',(-0.0714705827172459,0.300862454100803,
-1.09171050239691));
#35346=CARTESIAN_POINT('Ctrl Pts',(-0.0238235275724158,0.818068118928352,
-0.592123416550042));
#35347=CARTESIAN_POINT('Ctrl Pts',(0.,0.913908649078056,-0.288121577880454));
#35348=CARTESIAN_POINT('Origin',(-8.61687266823562,0.,0.));
#35349=CARTESIAN_POINT('',(-0.741872668235614,-0.956728983665432,-0.000237929659179223));
#35350=CARTESIAN_POINT('',(-0.653127331764369,-0.959131267467959,-0.000696535169553286));
#35351=CARTESIAN_POINT('',(-8.61687266823562,-0.95825,-1.32069628103871E-13));
#35352=CARTESIAN_POINT('Ctrl Pts',(-0.741872668235614,-0.956728983665433,
-0.000237929659179185));
#35353=CARTESIAN_POINT('Ctrl Pts',(-0.731052549154585,-0.957051776896419,
-0.145545400519289));
#35354=CARTESIAN_POINT('Ctrl Pts',(-0.696408902501142,-0.857684767529791,
-0.610369126283467));
#35355=CARTESIAN_POINT('Ctrl Pts',(-0.637941728275282,-0.135206620182443,
-1.12463688374277));
#35356=CARTESIAN_POINT('Ctrl Pts',(-0.566471145558034,0.87179625879392,
-0.723228026706244));
#35357=CARTESIAN_POINT('Ctrl Pts',(-0.495000562840788,1.08031370561788,
0.340570456675246));
#35358=CARTESIAN_POINT('Ctrl Pts',(-0.42352998012354,0.299404286128507,
1.09246172377618));
#35359=CARTESIAN_POINT('Ctrl Pts',(-0.355820681921817,-0.700244095450074,
0.856828377137249));
#35360=CARTESIAN_POINT('Ctrl Pts',(-0.31193491129251,-0.956624260471124,
0.267085417349426));
#35361=CARTESIAN_POINT('Ctrl Pts',(-0.291872668235618,-0.958947183310973,
-0.000747180795175641));
#35362=CARTESIAN_POINT('Ctrl Pts',(-0.653127331764369,-0.959131267467959,
-0.00069653516955346));
#35363=CARTESIAN_POINT('Ctrl Pts',(-0.649829969327988,-0.959491703395879,
-0.0446960802726476));
#35364=CARTESIAN_POINT('Ctrl Pts',(-0.62270907931919,-0.936746049792099,
-0.406219180022716));
#35365=CARTESIAN_POINT('Ctrl Pts',(-0.571764661737977,-0.477113298122812,
-1.02736478175254));
#35366=CARTESIAN_POINT('Ctrl Pts',(-0.50029407902073,0.604749195542173,
-0.957794082086403));
#35367=CARTESIAN_POINT('Ctrl Pts',(-0.428823496303482,1.1326255269949,-0.0110385894026361));
#35368=CARTESIAN_POINT('Ctrl Pts',(-0.357352913586236,0.623328692801092,
0.945926260653483));
#35369=CARTESIAN_POINT('Ctrl Pts',(-0.285882330868988,-0.457232996199784,
1.03633538397604));
#35370=CARTESIAN_POINT('Ctrl Pts',(-0.234473803595033,-0.932756597386936,
0.418887604268179));
#35371=CARTESIAN_POINT('Ctrl Pts',(-0.206888803893493,-0.959336606812183,
0.0510072686643281));
#35372=CARTESIAN_POINT('Ctrl Pts',(-0.203127331764369,-0.958925693334137,
0.000778823732210361));
#35373=CARTESIAN_POINT('Origin',(-8.61687266823562,0.,0.));
#35374=CARTESIAN_POINT('',(-1.19187266823562,-0.958088840212646,0.000876755735238218));
#35375=CARTESIAN_POINT('',(-1.10312733176437,-0.956784848343336,-0.000335004702462158));
#35376=CARTESIAN_POINT('',(-8.61687266823562,-0.95825,-1.32069628103871E-13));
#35377=CARTESIAN_POINT('Ctrl Pts',(-1.19187266823562,-0.958088840212646,
0.000876755735238132));
#35378=CARTESIAN_POINT('Ctrl Pts',(-1.17399371458908,-0.955922435214412,
-0.238368404924597));
#35379=CARTESIAN_POINT('Ctrl Pts',(-1.13229123337013,-0.744142554039245,
-0.799826227319725));
#35380=CARTESIAN_POINT('Ctrl Pts',(-1.06676522457877,0.1983703394913,-1.11522836645996));
#35381=CARTESIAN_POINT('Ctrl Pts',(-0.995294641861518,1.04470289737796,
-0.437813907286639));
#35382=CARTESIAN_POINT('Ctrl Pts',(-0.923824059144271,0.934198937671177,
0.640591100675686));
#35383=CARTESIAN_POINT('Ctrl Pts',(-0.852353476427024,-0.0319309011644629,
1.13228350740848));
#35384=CARTESIAN_POINT('Ctrl Pts',(-0.791703012790804,-0.82697889907382,
0.66948777117457));
#35385=CARTESIAN_POINT('Ctrl Pts',(-0.754876076727001,-0.956341057043799,
0.174389760322289));
#35386=CARTESIAN_POINT('Ctrl Pts',(-0.741872668235614,-0.956728983665433,
-0.000237929659179185));
#35387=CARTESIAN_POINT('Ctrl Pts',(-1.10312733176437,-0.956784848343336,
-0.000335004702462244));
#35388=CARTESIAN_POINT('Ctrl Pts',(-1.09277113476248,-0.957221115285983,
-0.139392137331314));
#35389=CARTESIAN_POINT('Ctrl Pts',(-1.05859141018818,-0.863731290477847,
-0.597779280961512));
#35390=CARTESIAN_POINT('Ctrl Pts',(-1.00058815804146,-0.157032780474456,
-1.12179595235208));
#35391=CARTESIAN_POINT('Ctrl Pts',(-0.929117575324211,0.857575021859809,
-0.740034212889895));
#35392=CARTESIAN_POINT('Ctrl Pts',(-0.857646992606967,1.0867335802145,0.31951868111913));
#35393=CARTESIAN_POINT('Ctrl Pts',(-0.786176409889718,0.320564368022132,
1.08642872230062));
#35394=CARTESIAN_POINT('Ctrl Pts',(-0.718003189608853,-0.690321369002484,
0.868807863254718));
#35395=CARTESIAN_POINT('Ctrl Pts',(-0.673653496900403,-0.956887544637908,
0.2732017535753));
#35396=CARTESIAN_POINT('Ctrl Pts',(-0.653127331764369,-0.959131267467959,
-0.00069653516955346));
#35397=CARTESIAN_POINT('Origin',(-8.61687266823562,0.,0.));
#35398=CARTESIAN_POINT('',(-1.64187266823562,-0.959728790079239,-0.000272255018208681));
#35399=CARTESIAN_POINT('',(-1.55312733176437,-0.957905508838967,0.000864921553367683));
#35400=CARTESIAN_POINT('',(-8.61687266823562,-0.95825,-1.32069628103871E-13));
#35401=CARTESIAN_POINT('Ctrl Pts',(-1.64187266823562,-0.959728790079238,
-0.000272255018208569));
#35402=CARTESIAN_POINT('Ctrl Pts',(-1.64075840759599,-0.959784665653602,
-0.0151165166273389));
#35403=CARTESIAN_POINT('Ctrl Pts',(-1.61582061938395,-0.95274448746835,
-0.347285402846716));
#35404=CARTESIAN_POINT('Ctrl Pts',(-1.5670593035995,-0.568921139707624,
-0.979496698268463));
#35405=CARTESIAN_POINT('Ctrl Pts',(-1.49558872088225,0.514728551628869,
-1.00902902087099));
#35406=CARTESIAN_POINT('Ctrl Pts',(-1.424118138165,1.12694188770285,-0.114398565074092));
#35407=CARTESIAN_POINT('Ctrl Pts',(-1.35264755544776,0.706996853826318,
0.885008749153142));
#35408=CARTESIAN_POINT('Ctrl Pts',(-1.28117697273051,-0.360481749440169,
1.07384261429556));
#35409=CARTESIAN_POINT('Ctrl Pts',(-1.22758534365979,-0.91335198538869,
0.477949908633713));
#35410=CARTESIAN_POINT('Ctrl Pts',(-1.1978172421615,-0.958809148286597,
0.0804233876057907));
#35411=CARTESIAN_POINT('Ctrl Pts',(-1.19187266823562,-0.958088840212646,
0.000876755735238132));
#35412=CARTESIAN_POINT('Ctrl Pts',(-1.55312733176437,-0.957905508838967,
0.000864921553367691));
#35413=CARTESIAN_POINT('Ctrl Pts',(-1.53571230019698,-0.955856605455542,
-0.232285840518138));
#35414=CARTESIAN_POINT('Ctrl Pts',(-1.49447374105717,-0.752915558634865,
-0.787577677013262));
#35415=CARTESIAN_POINT('Ctrl Pts',(-1.42941165434494,0.176662356954578,
-1.11887237535459));
#35416=CARTESIAN_POINT('Ctrl Pts',(-1.3579410716277,1.03599816963305,-0.458031427443242));
#35417=CARTESIAN_POINT('Ctrl Pts',(-1.28647048891045,0.946470301531875,
0.622317346917095));
#35418=CARTESIAN_POINT('Ctrl Pts',(-1.2149999061932,-0.00992315233657026,
1.13268996675844));
#35419=CARTESIAN_POINT('Ctrl Pts',(-1.15388552047784,-0.819962267279029,
0.682009929435178));
#35420=CARTESIAN_POINT('Ctrl Pts',(-1.1165946623349,-0.956217521250915,
0.180496662845114));
#35421=CARTESIAN_POINT('Ctrl Pts',(-1.10312733176437,-0.956784848343336,
-0.000335004702462244));
#35422=CARTESIAN_POINT('Origin',(-8.61687266823562,0.,0.));
#35423=CARTESIAN_POINT('',(-2.09187266823562,-0.957282800009966,-0.000711420515223326));
#35424=CARTESIAN_POINT('',(-2.00312733176437,-0.959789721040338,-0.000160985410693898));
#35425=CARTESIAN_POINT('',(-8.61687266823562,-0.95825,-1.32069628103871E-13));
#35426=CARTESIAN_POINT('Ctrl Pts',(-2.09187266823562,-0.957282800009966,
-0.000711420515223399));
#35427=CARTESIAN_POINT('Ctrl Pts',(-2.08369957303049,-0.958037494378474,
-0.110312090770477));
#35428=CARTESIAN_POINT('Ctrl Pts',(-2.05170295025294,-0.890024371399682,
-0.538476540815407));
#35429=CARTESIAN_POINT('Ctrl Pts',(-1.99588279990298,-0.258816672158623,
-1.10276877747064));
#35430=CARTESIAN_POINT('Ctrl Pts',(-1.92441221718573,0.786412695849304,
-0.815254633948207));
#35431=CARTESIAN_POINT('Ctrl Pts',(-1.85294163446849,1.11137205677529,0.218945650531032));
#35432=CARTESIAN_POINT('Ctrl Pts',(-1.78147105175124,0.418433355264041,
1.05261511171313));
#35433=CARTESIAN_POINT('Ctrl Pts',(-1.71111472967362,-0.640967447381487,
0.924234803949312));
#35434=CARTESIAN_POINT('Ctrl Pts',(-1.66458193516841,-0.958590014026201,
0.302262257387501));
#35435=CARTESIAN_POINT('Ctrl Pts',(-1.64187266823562,-0.959728790079238,
-0.000272255018208569));
#35436=CARTESIAN_POINT('Ctrl Pts',(-2.00312733176437,-0.959789721040338,
-0.000160985410693976));
#35437=CARTESIAN_POINT('Ctrl Pts',(-2.00247699320389,-0.959809874352138,
-0.00882337026222604));
#35438=CARTESIAN_POINT('Ctrl Pts',(-1.97800312707099,-0.955778669076828,
-0.334791339982387));
#35439=CARTESIAN_POINT('Ctrl Pts',(-1.92970573336567,-0.587846795790038,
-0.968256742613268));
#35440=CARTESIAN_POINT('Ctrl Pts',(-1.85823515064843,0.4950244060751,-1.01884042543795));
#35441=CARTESIAN_POINT('Ctrl Pts',(-1.78676456793118,1.12450614210672,-0.13627513368518));
#35442=CARTESIAN_POINT('Ctrl Pts',(-1.71529398521393,0.724060395961153,
0.871103620044959));
#35443=CARTESIAN_POINT('Ctrl Pts',(-1.64382340249668,-0.339547310642638,
1.08064452961661));
#35444=CARTESIAN_POINT('Ctrl Pts',(-1.58976785134683,-0.908777537601796,
0.490543016397207));
#35445=CARTESIAN_POINT('Ctrl Pts',(-1.55953582776939,-0.958659477564004,
0.0866612476479209));
#35446=CARTESIAN_POINT('Ctrl Pts',(-1.55312733176437,-0.957905508838967,
0.000864921553367691));
#35447=CARTESIAN_POINT('Origin',(-8.61687266823562,0.,0.));
#35448=CARTESIAN_POINT('',(-2.54187266823562,-0.957160045438329,0.000652648723329974));
#35449=CARTESIAN_POINT('',(-2.45312733176437,-0.957431559463739,-0.000767278543180316));
#35450=CARTESIAN_POINT('',(-8.61687266823562,-0.95825,-1.32069628103871E-13));
#35451=CARTESIAN_POINT('Ctrl Pts',(-2.54187266823562,-0.957160045438329,
0.000652648723330016));
#35452=CARTESIAN_POINT('Ctrl Pts',(-2.52664073846498,-0.955880301498824,
-0.203672381995242));
#35453=CARTESIAN_POINT('Ctrl Pts',(-2.48758528112193,-0.791644135614284,
-0.729450334203188));
#35454=CARTESIAN_POINT('Ctrl Pts',(-2.42470629620646,0.0737508650376029,
-1.13032997672338));
#35455=CARTESIAN_POINT('Ctrl Pts',(-2.35323571348922,0.989842956438803,
-0.550723131856308));
#35456=CARTESIAN_POINT('Ctrl Pts',(-2.28176513077197,0.999344656976215,
0.533287261191272));
#35457=CARTESIAN_POINT('Ctrl Pts',(-2.21029454805472,0.0935534241382057,
1.12886350069563));
#35458=CARTESIAN_POINT('Ctrl Pts',(-2.1469970605426,-0.784541427588874,
0.740648467365689));
#35459=CARTESIAN_POINT('Ctrl Pts',(-2.1075231006029,-0.955837656783825,
0.209159850305441));
#35460=CARTESIAN_POINT('Ctrl Pts',(-2.09187266823562,-0.957282800009966,
-0.000711420515223399));
#35461=CARTESIAN_POINT('Ctrl Pts',(-2.45312733176437,-0.957431559463739,
-0.000767278543180386));
#35462=CARTESIAN_POINT('Ctrl Pts',(-2.44541815863838,-0.958207306895283,
-0.104106321084798));
#35463=CARTESIAN_POINT('Ctrl Pts',(-2.41388545793998,-0.895165853018041,
-0.525871241247474));
#35464=CARTESIAN_POINT('Ctrl Pts',(-2.35852922966916,-0.280196248383438,
-1.09753133781927));
#35465=CARTESIAN_POINT('Ctrl Pts',(-2.28705864695191,0.770422572284684,
-0.830381861084687));
#35466=CARTESIAN_POINT('Ctrl Pts',(-2.21558806423466,1.11541663057547,0.197308680388403));
#35467=CARTESIAN_POINT('Ctrl Pts',(-2.14411748151742,0.438808229068046,
1.04428555155484));
#35468=CARTESIAN_POINT('Ctrl Pts',(-2.07329723736065,-0.62988784727845,
0.935804606318756));
#35469=CARTESIAN_POINT('Ctrl Pts',(-2.0263005207763,-0.959071608149721,
0.308501446215017));
#35470=CARTESIAN_POINT('Ctrl Pts',(-2.00312733176437,-0.959789721040338,
-0.000160985410693976));
#35471=CARTESIAN_POINT('Origin',(-8.61687266823562,0.,0.));
#35472=CARTESIAN_POINT('',(-2.99187266823562,-0.959650450245746,0.000368126650595699));
#35473=CARTESIAN_POINT('',(-2.90312733176437,-0.957038006623854,0.000579103131620948));
#35474=CARTESIAN_POINT('',(-8.61687266823562,-0.95825,-1.32069628103871E-13));
#35475=CARTESIAN_POINT('Ctrl Pts',(-2.99187266823562,-0.959650450245746,
0.000368126650595773));
#35476=CARTESIAN_POINT('Ctrl Pts',(-2.96958190389948,-0.958193208886187,
-0.296655628075332));
#35477=CARTESIAN_POINT('Ctrl Pts',(-2.92346761199092,-0.650782839392722,
-0.913731080697807));
#35478=CARTESIAN_POINT('Ctrl Pts',(-2.85352979250995,0.399917459173323,
-1.05978822045819));
#35479=CARTESIAN_POINT('Ctrl Pts',(-2.78205920979269,1.10736333094316,-0.238393581406989));
#35480=CARTESIAN_POINT('Ctrl Pts',(-2.71058862707545,0.800582704964894,
0.801344107662086));
#35481=CARTESIAN_POINT('Ctrl Pts',(-2.6391180443582,-0.239446142554869,
1.10713621166916));
#35482=CARTESIAN_POINT('Ctrl Pts',(-2.58287939141159,-0.885254315562734,
0.549848221345033));
#35483=CARTESIAN_POINT('Ctrl Pts',(-2.5504642660374,-0.957881887344315,
0.115902555413056));
#35484=CARTESIAN_POINT('Ctrl Pts',(-2.54187266823562,-0.957160045438329,
0.000652648723330016));
#35485=CARTESIAN_POINT('Ctrl Pts',(-2.90312733176437,-0.957038006623854,
0.000579103131620913));
#35486=CARTESIAN_POINT('Ctrl Pts',(-2.88835932407288,-0.955945717746202,
-0.197586125297776));
#35487=CARTESIAN_POINT('Ctrl Pts',(-2.84976778880897,-0.799342738306937,
-0.71701096012948));
#35488=CARTESIAN_POINT('Ctrl Pts',(-2.78735272597264,0.051772932289347,
-1.13154961826182));
#35489=CARTESIAN_POINT('Ctrl Pts',(-2.71588214325539,0.978954661287059,
-0.569853267298351));
#35490=CARTESIAN_POINT('Ctrl Pts',(-2.64441156053815,1.00951851444678,0.513767791999302));
#35491=CARTESIAN_POINT('Ctrl Pts',(-2.5729409778209,0.115471267790065,1.12683244602779));
#35492=CARTESIAN_POINT('Ctrl Pts',(-2.50917956822964,-0.776491202911252,
0.753033696487916));
#35493=CARTESIAN_POINT('Ctrl Pts',(-2.4692416862108,-0.955810027703003,
0.215240577611453));
#35494=CARTESIAN_POINT('Ctrl Pts',(-2.45312733176437,-0.957431559463739,
-0.000767278543180386));
#35495=CARTESIAN_POINT('Origin',(-8.61687266823562,0.,0.));
#35496=CARTESIAN_POINT('',(-3.44187266823562,-0.958257665410638,-0.000876459478439951));
#35497=CARTESIAN_POINT('',(-3.35312733176437,-0.959540833023362,0.000467762790667282));
#35498=CARTESIAN_POINT('',(-8.61687266823562,-0.95825,-1.32069628103871E-13));
#35499=CARTESIAN_POINT('Ctrl Pts',(-3.44187266823562,-0.958257665410638,
-0.00087645947844002));
#35500=CARTESIAN_POINT('Ctrl Pts',(-3.43634659690639,-0.958937642601644,
-0.0747896866542515));
#35501=CARTESIAN_POINT('Ctrl Pts',(-3.40699699800474,-0.917354581093434,
-0.466594412511799));
#35502=CARTESIAN_POINT('Ctrl Pts',(-3.35382387153068,-0.379250074662353,
-1.06735862166481));
#35503=CARTESIAN_POINT('Ctrl Pts',(-3.28235328881343,0.69137464498329,-0.897265928611934));
#35504=CARTESIAN_POINT('Ctrl Pts',(-3.21088270609618,1.12877405797548,0.0946264889719359));
#35505=CARTESIAN_POINT('Ctrl Pts',(-3.13941212337894,0.532337034832168,
0.999851152782103));
#35506=CARTESIAN_POINT('Ctrl Pts',(-3.06794154066169,-0.551663836031854,
0.989318987176647));
#35507=CARTESIAN_POINT('Ctrl Pts',(-3.01876172228058,-0.949899269571083,
0.358565498699607));
#35508=CARTESIAN_POINT('Ctrl Pts',(-2.99340543147189,-0.959750653448679,
0.0207921500119563));
#35509=CARTESIAN_POINT('Ctrl Pts',(-2.99187266823562,-0.959650450245746,
0.000368126650595773));
#35510=CARTESIAN_POINT('Ctrl Pts',(-3.35312733176437,-0.959540833023362,
0.000467762790667295));
#35511=CARTESIAN_POINT('Ctrl Pts',(-3.33130048950737,-0.957793875791413,
-0.290462270881725));
#35512=CARTESIAN_POINT('Ctrl Pts',(-3.28565011967796,-0.661465590816773,
-0.902016944463262));
#35513=CARTESIAN_POINT('Ctrl Pts',(-3.21617622227613,0.379248666114025,
-1.0673590887593));
#35514=CARTESIAN_POINT('Ctrl Pts',(-3.14470563955887,1.10252187493073,-0.259866293323276));
#35515=CARTESIAN_POINT('Ctrl Pts',(-3.07323505684163,0.816002842433735,
0.785636262049064));
#35516=CARTESIAN_POINT('Ctrl Pts',(-3.00176447412438,-0.217887610001112,
1.11157994067649));
#35517=CARTESIAN_POINT('Ctrl Pts',(-2.94506189909863,-0.879818475118968,
0.562453432935334));
#35518=CARTESIAN_POINT('Ctrl Pts',(-2.91218285164529,-0.957707781711591,
0.122091036442916));
#35519=CARTESIAN_POINT('Ctrl Pts',(-2.90312733176437,-0.957038006623854,
0.000579103131620913));
#35520=CARTESIAN_POINT('Origin',(-8.61687266823562,0.,0.));
#35521=CARTESIAN_POINT('',(-3.89187266823562,-0.956695459968737,0.000147939248303057));
#35522=CARTESIAN_POINT('',(-3.80312733176437,-0.958446399572106,-0.000863762433619825));
#35523=CARTESIAN_POINT('',(-8.61687266823562,-0.95825,-1.32069628103871E-13));
#35524=CARTESIAN_POINT('Ctrl Pts',(-3.89187266823562,-0.956695459968737,
0.000147939248303051));
#35525=CARTESIAN_POINT('Ctrl Pts',(-3.87928776234088,-0.956462580794984,
-0.168874488277431));
#35526=CARTESIAN_POINT('Ctrl Pts',(-3.84287932887373,-0.833157873073766,
-0.658177943823049));
#35527=CARTESIAN_POINT('Ctrl Pts',(-3.78264736783416,-0.0517744158194337,
-1.13154958187441));
#35528=CARTESIAN_POINT('Ctrl Pts',(-3.71117678511691,0.922826436408769,
-0.65686864336692));
#35529=CARTESIAN_POINT('Ctrl Pts',(-3.63970620239967,1.05221686991099,0.419433791018696));
#35530=CARTESIAN_POINT('Ctrl Pts',(-3.56823561968242,0.217889071988309,
1.11157968615915));
#35531=CARTESIAN_POINT('Ctrl Pts',(-3.50229110829441,-0.7360618847371,0.810839058251395));
#35532=CARTESIAN_POINT('Ctrl Pts',(-3.4601701244788,-0.956006182909324,
0.243858716647063));
#35533=CARTESIAN_POINT('Ctrl Pts',(-3.44187266823562,-0.958257665410638,
-0.00087645947844002));
#35534=CARTESIAN_POINT('Ctrl Pts',(-3.80312733176437,-0.958446399572106,
-0.000863762433619868));
#35535=CARTESIAN_POINT('Ctrl Pts',(-3.79806518251428,-0.959072080853087,
-0.0685377004959773));
#35536=CARTESIAN_POINT('Ctrl Pts',(-3.76917950569178,-0.921655890668159,
-0.454012480968252));
#35537=CARTESIAN_POINT('Ctrl Pts',(-3.71647030129686,-0.399918836166434,
-1.05978766721718));
#35538=CARTESIAN_POINT('Ctrl Pts',(-3.6449997185796,0.673808865727154,-0.910530937186564));
#35539=CARTESIAN_POINT('Ctrl Pts',(-3.57352913586236,1.13039963799526,0.072674847963582));
#35540=CARTESIAN_POINT('Ctrl Pts',(-3.50205855314511,0.551665116510674,
0.989318237136875));
#35541=CARTESIAN_POINT('Ctrl Pts',(-3.43058797042786,-0.532335710452797,
0.999851822263215));
#35542=CARTESIAN_POINT('Ctrl Pts',(-3.38094422996762,-0.946623962906586,
0.371079864210543));
#35543=CARTESIAN_POINT('Ctrl Pts',(-3.35512401707979,-0.959700641932531,
0.0270815862291171));
#35544=CARTESIAN_POINT('Ctrl Pts',(-3.35312733176437,-0.959540833023362,
0.000467762790667295));
#35545=CARTESIAN_POINT('Origin',(-8.61687266823562,0.,0.));
#35546=CARTESIAN_POINT('',(-4.34187266823562,-0.958801047132561,0.000803658998405769));
#35547=CARTESIAN_POINT('',(-4.25312733176437,-0.956676639742279,4.61738887314045E-5));
#35548=CARTESIAN_POINT('',(-8.61687266823562,-0.95825,-1.32069628103871E-13));
#35549=CARTESIAN_POINT('Ctrl Pts',(-4.34187266823562,-0.958801047132561,
0.000803658998405725));
#35550=CARTESIAN_POINT('Ctrl Pts',(-4.32222892777538,-0.956446580846668,
-0.261555840640749));
#35551=CARTESIAN_POINT('Ctrl Pts',(-4.27876165974272,-0.708980756137565,
-0.846004557974328));
#35552=CARTESIAN_POINT('Ctrl Pts',(-4.21147086413764,0.280194818630884,
-1.09753173529789));
#35553=CARTESIAN_POINT('Ctrl Pts',(-4.1400002814204,1.07418480140191,-0.359460788975286));
#35554=CARTESIAN_POINT('Ctrl Pts',(-4.06852969870314,0.884336274609667,
0.707837834382355));
#35555=CARTESIAN_POINT('Ctrl Pts',(-3.99705911598591,-0.115469795083229,
1.12683262856426));
#35556=CARTESIAN_POINT('Ctrl Pts',(-3.93817343916339,-0.85208931007107,
0.621720486442062));
#35557=CARTESIAN_POINT('Ctrl Pts',(-3.9031112899133,-0.956903426635498,
0.151089005784113));
#35558=CARTESIAN_POINT('Ctrl Pts',(-3.89187266823562,-0.956695459968737,
0.000147939248303051));
#35559=CARTESIAN_POINT('Ctrl Pts',(-4.25312733176437,-0.956676639742279,
4.61738887314392E-5));
#35560=CARTESIAN_POINT('Ctrl Pts',(-4.24100634794878,-0.956606710883735,
-0.162753489137796));
#35561=CARTESIAN_POINT('Ctrl Pts',(-4.20506183656076,-0.839843493636197,
-0.645626437601176));
#35562=CARTESIAN_POINT('Ctrl Pts',(-4.14529379760033,-0.0737523434839011,
-1.1303298487331));
#35563=CARTESIAN_POINT('Ctrl Pts',(-4.07382321488309,0.909888230063614,
-0.674676503146548));
#35564=CARTESIAN_POINT('Ctrl Pts',(-4.00235263216584,1.06016839954784,0.398908435241142));
#35565=CARTESIAN_POINT('Ctrl Pts',(-3.93088204944859,0.239447586020594,
1.1071358672969));
#35566=CARTESIAN_POINT('Ctrl Pts',(-3.86447361598144,-0.726917995153459,
0.823003811913429));
#35567=CARTESIAN_POINT('Ctrl Pts',(-3.8218887100867,-0.956127494569163,
0.249949931873536));
#35568=CARTESIAN_POINT('Ctrl Pts',(-3.80312733176437,-0.958446399572106,
-0.000863762433619868));
#35569=CARTESIAN_POINT('Origin',(-8.61687266823562,0.,0.));
#35570=CARTESIAN_POINT('',(-4.79187266823562,-0.959278083226344,-0.00063277652707348));
#35571=CARTESIAN_POINT('',(-4.70312733176437,-0.958616057498963,0.000841104330781481));
#35572=CARTESIAN_POINT('',(-8.61687266823562,-0.95825,-1.32069628103871E-13));
#35573=CARTESIAN_POINT('Ctrl Pts',(-4.79187266823562,-0.959278083226344,
-0.000632776527073604));
#35574=CARTESIAN_POINT('Ctrl Pts',(-4.78899362078229,-0.959570967253412,
-0.0390352664624121));
#35575=CARTESIAN_POINT('Ctrl Pts',(-4.76229104575654,-0.940036834855403,
-0.394909991490227));
#35576=CARTESIAN_POINT('Ctrl Pts',(-4.71176494315838,-0.495025754436958,
-1.01883980527742));
#35577=CARTESIAN_POINT('Ctrl Pts',(-4.64029436044113,0.587845543979899,
-0.968257539498959));
#35578=CARTESIAN_POINT('Ctrl Pts',(-4.56882377772388,1.13231313096107,-0.0308548185336372));
#35579=CARTESIAN_POINT('Ctrl Pts',(-4.49735319500663,0.639702869075108,
0.934807619604525));
#35580=CARTESIAN_POINT('Ctrl Pts',(-4.42588261228939,-0.438806873470812,
1.0442861553082));
#35581=CARTESIAN_POINT('Ctrl Pts',(-4.37405577003238,-0.92944979296497,
0.430102104777608));
#35582=CARTESIAN_POINT('Ctrl Pts',(-4.34605245534779,-0.959302029512049,
0.0566284067121712));
#35583=CARTESIAN_POINT('Ctrl Pts',(-4.34187266823562,-0.958801047132561,
0.000803658998405725));
#35584=CARTESIAN_POINT('Ctrl Pts',(-4.70312733176437,-0.958616057498963,
0.000841104330781481));
#35585=CARTESIAN_POINT('Ctrl Pts',(-4.68394751338327,-0.956263924788962,
-0.255449887934941));
#35586=CARTESIAN_POINT('Ctrl Pts',(-4.64094416742975,-0.718501334310948,
-0.833934531383708));
#35587=CARTESIAN_POINT('Ctrl Pts',(-4.57411729390382,0.258815220585386,
-1.10276908584694));
#35588=CARTESIAN_POINT('Ctrl Pts',(-4.50264671118657,1.06699709340334,-0.380265930337164));
#35589=CARTESIAN_POINT('Ctrl Pts',(-4.43117612846933,0.897923629232473,
0.690520188823135));
#35590=CARTESIAN_POINT('Ctrl Pts',(-4.35970554575208,-0.093551942967458,
1.12886359188051));
#35591=CARTESIAN_POINT('Ctrl Pts',(-4.30035594685043,-0.845727021412224,
0.634294523148357));
#35592=CARTESIAN_POINT('Ctrl Pts',(-4.26482987552119,-0.956744154519911,
0.157225674261628));
#35593=CARTESIAN_POINT('Ctrl Pts',(-4.25312733176437,-0.956676639742279,
4.61738887314392E-5));
#35594=CARTESIAN_POINT('Origin',(-8.61687266823562,0.,0.));
#35595=CARTESIAN_POINT('',(-5.24187266823562,-0.956851161348753,-0.000418646029398152));
#35596=CARTESIAN_POINT('',(-5.15312733176438,-0.959424157494653,-0.000550396959753813));
#35597=CARTESIAN_POINT('',(-8.61687266823562,-0.95825,-1.32069628103871E-13));
#35598=CARTESIAN_POINT('Ctrl Pts',(-5.24187266823562,-0.956851161348753,
-0.000418646029398334));
#35599=CARTESIAN_POINT('Ctrl Pts',(-5.23193478621678,-0.957376403620873,
-0.133835808799005));
#35600=CARTESIAN_POINT('Ctrl Pts',(-5.19817337662553,-0.869043093986714,
-0.586421640241982));
#35601=CARTESIAN_POINT('Ctrl Pts',(-5.14058843946185,-0.176663834249519,
-1.11887217144864));
#35602=CARTESIAN_POINT('Ctrl Pts',(-5.06911785674461,0.844476313709149,
-0.754946886845504));
#35603=CARTESIAN_POINT('Ctrl Pts',(-4.99764727402736,1.09216638421668,0.30042908574342));
#35604=CARTESIAN_POINT('Ctrl Pts',(-4.92617669131012,0.339548736498745,
1.08064411436687));
#35605=CARTESIAN_POINT('Ctrl Pts',(-4.8575851560462,-0.681213984298933,
0.879545467471477));
#35606=CARTESIAN_POINT('Ctrl Pts',(-4.8128171483547,-0.957147411960396,
0.278737466586754));
#35607=CARTESIAN_POINT('Ctrl Pts',(-4.79187266823562,-0.959278083226344,
-0.000632776527073604));
#35608=CARTESIAN_POINT('Ctrl Pts',(-5.15312733176438,-0.959424157494653,
-0.00055039695975393));
#35609=CARTESIAN_POINT('Ctrl Pts',(-5.15071220639018,-0.95964469725191,
-0.0327519345529813));
#35610=CARTESIAN_POINT('Ctrl Pts',(-5.12447355344357,-0.943559089128387,
-0.382376225977263));
#35611=CARTESIAN_POINT('Ctrl Pts',(-5.07441137292454,-0.514729859854887,
-1.00902831797734));
#35612=CARTESIAN_POINT('Ctrl Pts',(-5.00294079020731,0.56891984144925,-0.979497416592661));
#35613=CARTESIAN_POINT('Ctrl Pts',(-4.93147020749005,1.13149975276759,-0.0528515334991769));
#35614=CARTESIAN_POINT('Ctrl Pts',(-4.85999962477281,0.657746782740738,
0.92220070749299));
#35615=CARTESIAN_POINT('Ctrl Pts',(-4.78852904205556,-0.418431965008117,
1.05261563059162));
#35616=CARTESIAN_POINT('Ctrl Pts',(-4.73623827771942,-0.925414685010962,
0.442670069694638));
#35617=CARTESIAN_POINT('Ctrl Pts',(-4.70777104095569,-0.959185542572679,
0.0628928304100949));
#35618=CARTESIAN_POINT('Ctrl Pts',(-4.70312733176437,-0.958616057498963,
0.000841104330781481));
#35619=CARTESIAN_POINT('Origin',(-8.61687266823562,0.,0.));
#35620=CARTESIAN_POINT('',(-5.69187266823562,-0.957745541375101,0.000843587520472362));
#35621=CARTESIAN_POINT('',(-5.60312733176437,-0.956941681982296,-0.000506047312858471));
#35622=CARTESIAN_POINT('',(-8.61687266823562,-0.95825,-1.32069628103871E-13));
#35623=CARTESIAN_POINT('Ctrl Pts',(-5.69187266823562,-0.957745541375101,
0.00084358752047234));
#35624=CARTESIAN_POINT('Ctrl Pts',(-5.67487595165128,-0.955820359152125,
-0.226803304052992));
#35625=CARTESIAN_POINT('Ctrl Pts',(-5.63405570749452,-0.760661038176944,
-0.776499075945558));
#35626=CARTESIAN_POINT('Ctrl Pts',(-5.56941193576534,0.157030992812372,
-1.1217960214248));
#35627=CARTESIAN_POINT('Ctrl Pts',(-5.49794135304809,1.02781377622821,-0.476113313998863));
#35628=CARTESIAN_POINT('Ctrl Pts',(-5.42647077033084,0.957228954744552,
0.605638319931491));
#35629=CARTESIAN_POINT('Ctrl Pts',(-5.3550001876136,0.00992468338927851,
1.13268996068449));
#35630=CARTESIAN_POINT('Ctrl Pts',(-5.29346748691519,-0.813484292874832,
0.69328502015914));
#35631=CARTESIAN_POINT('Ctrl Pts',(-5.2557583137892,-0.956117269760326,
0.185997677838279));
#35632=CARTESIAN_POINT('Ctrl Pts',(-5.24187266823562,-0.956851161348753,
-0.000418646029398334));
#35633=CARTESIAN_POINT('Ctrl Pts',(-5.60312733176437,-0.956941681982296,
-0.000506047312858627));
#35634=CARTESIAN_POINT('Ctrl Pts',(-5.59365337182468,-0.957550312161305,
-0.127664896619225));
#35635=CARTESIAN_POINT('Ctrl Pts',(-5.56035588431256,-0.874780422660147,
-0.573821257585252));
#35636=CARTESIAN_POINT('Ctrl Pts',(-5.50323486922804,-0.198371837060489,
-1.11522804366184));
#35637=CARTESIAN_POINT('Ctrl Pts',(-5.43176428651079,0.829647095487569,
-0.771213765472918));
#35638=CARTESIAN_POINT('Ctrl Pts',(-5.36029370379354,1.09779793008511,0.279149923530103));
#35639=CARTESIAN_POINT('Ctrl Pts',(-5.28882312107629,0.360483152130068,
1.07384210763829));
#35640=CARTESIAN_POINT('Ctrl Pts',(-5.21976766373324,-0.670923561447508,
0.89139065675279));
#35641=CARTESIAN_POINT('Ctrl Pts',(-5.1745357339626,-0.957469226345113,
0.28489377731112));
#35642=CARTESIAN_POINT('Ctrl Pts',(-5.15312733176438,-0.959424157494653,
-0.00055039695975393));
#35643=CARTESIAN_POINT('Origin',(-8.61687266823562,0.,0.));
#35644=CARTESIAN_POINT('',(-6.14187266823562,-0.959818611724535,-5.7784059915537E-5));
#35645=CARTESIAN_POINT('',(-6.05312733176438,-0.957575902522396,0.000808576896546773));
#35646=CARTESIAN_POINT('',(-8.61687266823562,-0.95825,-1.32069628103871E-13));
#35647=CARTESIAN_POINT('Ctrl Pts',(-6.14187266823562,-0.959818611724535,
-5.77840599154589E-5));
#35648=CARTESIAN_POINT('Ctrl Pts',(-6.14164064465819,-0.95982130723207,
-0.0031480436667598));
#35649=CARTESIAN_POINT('Ctrl Pts',(-6.11758509350833,-0.958407877072966,
-0.323534921547347));
#35650=CARTESIAN_POINT('Ctrl Pts',(-6.06970601478608,-0.604721823700482,
-0.957808206827138));
#35651=CARTESIAN_POINT('Ctrl Pts',(-5.99823543206882,0.47709687534022,-1.02735759037585));
#35652=CARTESIAN_POINT('Ctrl Pts',(-5.92676484935158,1.12194581094373,-0.155957185437944));
#35653=CARTESIAN_POINT('Ctrl Pts',(-5.85529426663432,0.739212255050342,
0.858283337941351));
#35654=CARTESIAN_POINT('Ctrl Pts',(-5.78382368391709,-0.320560747180587,
1.08642802515142));
#35655=CARTESIAN_POINT('Ctrl Pts',(-5.72934981778418,-0.904527421769531,
0.501902134781091));
#35656=CARTESIAN_POINT('Ctrl Pts',(-5.69869947922369,-0.958518799850562,
0.0922790299532361));
#35657=CARTESIAN_POINT('Ctrl Pts',(-5.69187266823562,-0.957745541375101,
0.00084358752047234));
#35658=CARTESIAN_POINT('Ctrl Pts',(-6.05312733176438,-0.957575902522396,
0.000808576896546643));
#35659=CARTESIAN_POINT('Ctrl Pts',(-6.03659453725917,-0.95580418331262,
-0.220724011270484));
#35660=CARTESIAN_POINT('Ctrl Pts',(-5.99623821518156,-0.769069431346248,
-0.764177221634974));
#35661=CARTESIAN_POINT('Ctrl Pts',(-5.93205836553151,0.135203161210182,
-1.12463553224998));
#35662=CARTESIAN_POINT('Ctrl Pts',(-5.86058778281427,1.01836809138401,-0.495995368476964));
#35663=CARTESIAN_POINT('Ctrl Pts',(-5.78911720009702,0.968816654749839,
0.586923559386877));
#35664=CARTESIAN_POINT('Ctrl Pts',(-5.71764661737977,0.0319326731109062,
1.13228321523766));
#35665=CARTESIAN_POINT('Ctrl Pts',(-5.65564999460223,-0.806130353491351,
0.705769711573949));
#35666=CARTESIAN_POINT('Ctrl Pts',(-5.61747689939709,-0.956019830932409,
0.192092878567596));
#35667=CARTESIAN_POINT('Ctrl Pts',(-5.60312733176437,-0.956941681982296,
-0.000506047312858627));
#35668=CARTESIAN_POINT('Origin',(-8.61687266823562,0.,0.));
#35669=CARTESIAN_POINT('',(-6.59187266823562,-0.957575883836689,-0.000808561082841419));
#35670=CARTESIAN_POINT('',(-6.50312733176438,-0.959818590364428,5.77507014088265E-5));
#35671=CARTESIAN_POINT('',(-8.61687266823562,-0.95825,-1.32069628103871E-13));
#35672=CARTESIAN_POINT('Ctrl Pts',(-6.59187266823562,-0.957575883836689,
-0.000808561082841245));
#35673=CARTESIAN_POINT('Ctrl Pts',(-6.58458181009268,-0.958357188928375,
-0.0985030576430004));
#35674=CARTESIAN_POINT('Ctrl Pts',(-6.55346742437732,-0.899671699226215,
-0.514506640016404));
#35675=CARTESIAN_POINT('Ctrl Pts',(-6.49852951108958,-0.299383568459973,
-1.09245341423609));
#35676=CARTESIAN_POINT('Ctrl Pts',(-6.42705892837228,0.755754835285377,
-0.843753338464662));
#35677=CARTESIAN_POINT('Ctrl Pts',(-6.35558834565508,1.11870256511677,0.177734697675315));
#35678=CARTESIAN_POINT('Ctrl Pts',(-6.28411776293779,0.457038265720188,
1.03643671348781));
#35679=CARTESIAN_POINT('Ctrl Pts',(-6.21287920379801,-0.6197172650586,0.946167455774252));
#35680=CARTESIAN_POINT('Ctrl Pts',(-6.1654641722306,-0.959544540108726,
0.314151110856649));
#35681=CARTESIAN_POINT('Ctrl Pts',(-6.14187266823562,-0.959818611724535,
-5.77840599154589E-5));
#35682=CARTESIAN_POINT('Ctrl Pts',(-6.50312733176438,-0.959818590364428,
5.77507014088167E-5));
#35683=CARTESIAN_POINT('Ctrl Pts',(-6.47953570269367,-0.959544661648279,
-0.314152798513479));
#35684=CARTESIAN_POINT('Ctrl Pts',(-6.43212054605054,-0.619714180231002,
-0.94617051184503));
#35685=CARTESIAN_POINT('Ctrl Pts',(-6.360881861835,0.457043683047776,-1.03643429626688));
#35686=CARTESIAN_POINT('Ctrl Pts',(-6.28941127911776,1.11870346430575,-0.177728822944574));
#35687=CARTESIAN_POINT('Ctrl Pts',(-6.2179406964005,0.755750395960032,0.843757259442018));
#35688=CARTESIAN_POINT('Ctrl Pts',(-6.14647011368326,-0.299389288185346,
1.09245184324826));
#35689=CARTESIAN_POINT('Ctrl Pts',(-6.09153232547121,-0.899672997516219,
0.514503194076797));
#35690=CARTESIAN_POINT('Ctrl Pts',(-6.06041806483159,-0.958357206120191,
0.098501375624914));
#35691=CARTESIAN_POINT('Ctrl Pts',(-6.05312733176438,-0.957575902522396,
0.000808576896546643));
#35692=CARTESIAN_POINT('Origin',(-8.61687266823562,0.,0.));
#35693=CARTESIAN_POINT('',(-7.04187266823562,-0.956941536305503,0.000507261239360324));
#35694=CARTESIAN_POINT('',(-6.95312733176437,-0.957745460096,-0.000843557184232457));
#35695=CARTESIAN_POINT('',(-8.61687266823562,-0.95825,-1.32069628103871E-13));
#35696=CARTESIAN_POINT('Ctrl Pts',(-7.04187266823562,-0.956941536305503,
0.000507261239360299));
#35697=CARTESIAN_POINT('Ctrl Pts',(-7.02752297552718,-0.956019718516196,
-0.19209383932285));
#35698=CARTESIAN_POINT('Ctrl Pts',(-6.98934975524631,-0.806128695492176,
-0.705775048482281));
#35699=CARTESIAN_POINT('Ctrl Pts',(-6.92735300739304,0.0319388218506953,
-1.1322817885948));
#35700=CARTESIAN_POINT('Ctrl Pts',(-6.85588242467578,0.968819643033635,
-0.586919179874541));
#35701=CARTESIAN_POINT('Ctrl Pts',(-6.78441184195855,1.0183655808885,0.496001075865819));
#35702=CARTESIAN_POINT('Ctrl Pts',(-6.71294125924129,0.135197241307266,
1.12463608307476));
#35703=CARTESIAN_POINT('Ctrl Pts',(-6.648761534667,-0.769071682396365,0.764173986137034));
#35704=CARTESIAN_POINT('Ctrl Pts',(-6.60840533766509,-0.955804205036859,
0.220722400710996));
#35705=CARTESIAN_POINT('Ctrl Pts',(-6.59187266823562,-0.957575883836689,
-0.000808561082841245));
#35706=CARTESIAN_POINT('Ctrl Pts',(-6.95312733176437,-0.957745460096,-0.000843557184232414));
#35707=CARTESIAN_POINT('Ctrl Pts',(-6.94630039570057,-0.958518738839012,
-0.0922807305074193));
#35708=CARTESIAN_POINT('Ctrl Pts',(-6.91564993206436,-0.904526183542863,
-0.501905736657279));
#35709=CARTESIAN_POINT('Ctrl Pts',(-6.86117594085573,-0.32055498375887,
-1.08642949326629));
#35710=CARTESIAN_POINT('Ctrl Pts',(-6.78970535813849,0.739216698253442,
-0.858279536751942));
#35711=CARTESIAN_POINT('Ctrl Pts',(-6.71823477542123,1.12194498002037,0.155963109595212));
#35712=CARTESIAN_POINT('Ctrl Pts',(-6.64676419270399,0.477091470497689,
1.02736003461986));
#35713=CARTESIAN_POINT('Ctrl Pts',(-6.57529360998674,-0.604726820287475,
0.957805026523516));
#35714=CARTESIAN_POINT('Ctrl Pts',(-6.5274146563402,-0.958408621577299,
0.323531547364598));
#35715=CARTESIAN_POINT('Ctrl Pts',(-6.50335923026608,-0.959821282999966,
0.00314634434472348));
#35716=CARTESIAN_POINT('Ctrl Pts',(-6.50312733176438,-0.959818590364428,
5.77507014088167E-5));
#35717=CARTESIAN_POINT('Origin',(-8.61687266823562,0.,0.));
#35718=CARTESIAN_POINT('',(-7.49187266823562,-0.959412934693052,0.000617836956614901));
#35719=CARTESIAN_POINT('',(-7.40312733176438,-0.956848572177365,0.000426154272836141));
#35720=CARTESIAN_POINT('',(-8.61687266823562,-0.95825,-1.32069628103871E-13));
#35721=CARTESIAN_POINT('Ctrl Pts',(-7.49187266823563,-0.959412934693052,
0.000617836956614886));
#35722=CARTESIAN_POINT('Ctrl Pts',(-7.47046414096167,-0.95745509653909,
-0.284810027720839));
#35723=CARTESIAN_POINT('Ctrl Pts',(-7.4252320861153,-0.670938943283241,
-0.891502624484874));
#35724=CARTESIAN_POINT('Ctrl Pts',(-7.35617650369652,0.360498878016349,
-1.07377985091759));
#35725=CARTESIAN_POINT('Ctrl Pts',(-7.28470592097927,1.09779410779162,-0.279175995659392));
#35726=CARTESIAN_POINT('Ctrl Pts',(-7.21323533826203,0.829645878065874,
0.771234893840035));
#35727=CARTESIAN_POINT('Ctrl Pts',(-7.14176475554478,-0.198379160483441,
1.11521820608871));
#35728=CARTESIAN_POINT('Ctrl Pts',(-7.08464386553598,-0.874781647304231,
0.573819820530738));
#35729=CARTESIAN_POINT('Ctrl Pts',(-7.05134650309959,-0.957550131185408,
0.127664759202453));
#35730=CARTESIAN_POINT('Ctrl Pts',(-7.04187266823562,-0.956941536305503,
0.000507261239360299));
#35731=CARTESIAN_POINT('Ctrl Pts',(-7.40312733176438,-0.956848572177365,
0.000426154272836167));
#35732=CARTESIAN_POINT('Ctrl Pts',(-7.38924156113507,-0.956115802214307,
-0.185995226131067));
#35733=CARTESIAN_POINT('Ctrl Pts',(-7.35153226293335,-0.813486685078433,
-0.693301032778434));
#35734=CARTESIAN_POINT('Ctrl Pts',(-7.28999943715921,0.00993354252272871,
-1.13268140760685));
#35735=CARTESIAN_POINT('Ctrl Pts',(-7.21852885444197,0.95723056012177,-0.605637750215496));
#35736=CARTESIAN_POINT('Ctrl Pts',(-7.14705827172472,1.02781206513943,0.476121036543225));
#35737=CARTESIAN_POINT('Ctrl Pts',(-7.07558768900747,0.157024683432387,
1.12179557439976));
#35738=CARTESIAN_POINT('Ctrl Pts',(-7.01094404235403,-0.760663146684144,
0.776496209154286));
#35739=CARTESIAN_POINT('Ctrl Pts',(-6.97012392327299,-0.95582027685209,
0.226801797796848));
#35740=CARTESIAN_POINT('Ctrl Pts',(-6.95312733176437,-0.957745460096,-0.000843557184232414));
#35741=CARTESIAN_POINT('Ctrl Pts',(-7.93323468161444,-0.418777734804018,
0.861898063191011));
#35742=CARTESIAN_POINT('Ctrl Pts',(-7.90941115404202,-0.705478813976586,
0.722596173989356));
#35743=CARTESIAN_POINT('Ctrl Pts',(-7.86176409889719,-1.12398839549112,
0.137840937796296));
#35744=CARTESIAN_POINT('Ctrl Pts',(-7.79029351617994,-0.724317328358726,
-0.871877473921692));
#35745=CARTESIAN_POINT('Ctrl Pts',(-7.7188229334627,0.339691526025321,-1.08024419838854));
#35746=CARTESIAN_POINT('Ctrl Pts',(-7.64735235074545,1.09209582283259,-0.300632258159738));
#35747=CARTESIAN_POINT('Ctrl Pts',(-7.5758817680282,0.844510306117659,0.755061250975084));
#35748=CARTESIAN_POINT('Ctrl Pts',(-7.50441118531095,-0.17668969425852,
1.11881329398577));
#35749=CARTESIAN_POINT('Ctrl Pts',(-7.43294060259371,-1.03599061787127,
0.458055163568042));
#35750=CARTESIAN_POINT('Ctrl Pts',(-7.36147001987646,-0.946471802875193,
-0.62233963427798));
#35751=CARTESIAN_POINT('Ctrl Pts',(-7.28999943715921,0.00993354252272871,
-1.13268140760685));
#35752=CARTESIAN_POINT('Ctrl Pts',(-7.21852885444197,0.95723056012177,-0.605637750215496));
#35753=CARTESIAN_POINT('Ctrl Pts',(-7.14705827172472,1.02781206513943,0.476121036543225));
#35754=CARTESIAN_POINT('Ctrl Pts',(-7.07558768900747,0.157024683432387,
1.12179557439976));
#35755=CARTESIAN_POINT('Ctrl Pts',(-7.00411710629023,-0.857579030410797,
0.740029567628956));
#35756=CARTESIAN_POINT('Ctrl Pts',(-6.93264652357297,-1.08673276902163,
-0.319526746285243));
#35757=CARTESIAN_POINT('Ctrl Pts',(-6.86117594085573,-0.32055498375887,
-1.08642949326629));
#35758=CARTESIAN_POINT('Ctrl Pts',(-6.78970535813849,0.739216698253442,
-0.858279536751942));
#35759=CARTESIAN_POINT('Ctrl Pts',(-6.71823477542123,1.12194498002037,0.155963109595212));
#35760=CARTESIAN_POINT('Ctrl Pts',(-6.64676419270399,0.477091470497689,
1.02736003461986));
#35761=CARTESIAN_POINT('Ctrl Pts',(-6.57529360998674,-0.604726820287475,
0.957805026523516));
#35762=CARTESIAN_POINT('Ctrl Pts',(-6.50382302726949,-1.1326799710869,0.0110028993876029));
#35763=CARTESIAN_POINT('Ctrl Pts',(-6.43235244455225,-0.623219277748515,
-0.94587668221305));
#35764=CARTESIAN_POINT('Ctrl Pts',(-6.360881861835,0.457043683047776,-1.03643429626688));
#35765=CARTESIAN_POINT('Ctrl Pts',(-6.28941127911776,1.11870346430575,-0.177728822944574));
#35766=CARTESIAN_POINT('Ctrl Pts',(-6.2179406964005,0.755750395960032,0.843757259442018));
#35767=CARTESIAN_POINT('Ctrl Pts',(-6.14647011368326,-0.299389288185346,
1.09245184324826));
#35768=CARTESIAN_POINT('Ctrl Pts',(-6.07499953096601,-1.08032037219545,
0.340577257808081));
#35769=CARTESIAN_POINT('Ctrl Pts',(-6.00352894824877,-0.871793419144197,
-0.72322970712875));
#35770=CARTESIAN_POINT('Ctrl Pts',(-5.93205836553151,0.135203161210182,
-1.12463553224998));
#35771=CARTESIAN_POINT('Ctrl Pts',(-5.86058778281427,1.01836809138401,-0.495995368476964));
#35772=CARTESIAN_POINT('Ctrl Pts',(-5.78911720009702,0.968816654749839,
0.586923559386877));
#35773=CARTESIAN_POINT('Ctrl Pts',(-5.71764661737977,0.0319326731109062,
1.13228321523766));
#35774=CARTESIAN_POINT('Ctrl Pts',(-5.64617603466253,-0.934198225340768,
0.640592421805296));
#35775=CARTESIAN_POINT('Ctrl Pts',(-5.57470545194528,-1.04470336139031,
-0.437812587534104));
#35776=CARTESIAN_POINT('Ctrl Pts',(-5.50323486922804,-0.198371837060489,
-1.11522804366184));
#35777=CARTESIAN_POINT('Ctrl Pts',(-5.43176428651079,0.829647095487569,
-0.771213765472918));
#35778=CARTESIAN_POINT('Ctrl Pts',(-5.36029370379354,1.09779793008511,0.279149923530103));
#35779=CARTESIAN_POINT('Ctrl Pts',(-5.28882312107629,0.360483152130068,
1.07384210763829));
#35780=CARTESIAN_POINT('Ctrl Pts',(-5.21735253835905,-0.706995678278174,
0.885009653055967));
#35781=CARTESIAN_POINT('Ctrl Pts',(-5.1458819556418,-1.12694200452402,-0.114397087138167));
#35782=CARTESIAN_POINT('Ctrl Pts',(-5.07441137292454,-0.514729859854887,
-1.00902831797734));
#35783=CARTESIAN_POINT('Ctrl Pts',(-5.00294079020731,0.56891984144925,-0.979497416592661));
#35784=CARTESIAN_POINT('Ctrl Pts',(-4.93147020749005,1.13149975276759,-0.0528515334991769));
#35785=CARTESIAN_POINT('Ctrl Pts',(-4.85999962477281,0.657746782740738,
0.92220070749299));
#35786=CARTESIAN_POINT('Ctrl Pts',(-4.78852904205556,-0.418431965008117,
1.05261563059162));
#35787=CARTESIAN_POINT('Ctrl Pts',(-4.71705845933831,-1.11137173909997,
0.218947100086459));
#35788=CARTESIAN_POINT('Ctrl Pts',(-4.64558787662107,-0.786413741840137,
-0.815253581256376));
#35789=CARTESIAN_POINT('Ctrl Pts',(-4.57411729390382,0.258815220585386,
-1.10276908584694));
#35790=CARTESIAN_POINT('Ctrl Pts',(-4.50264671118657,1.06699709340334,-0.380265930337164));
#35791=CARTESIAN_POINT('Ctrl Pts',(-4.43117612846933,0.897923629232473,
0.690520188823135));
#35792=CARTESIAN_POINT('Ctrl Pts',(-4.35970554575208,-0.093551942967458,
1.12886359188051));
#35793=CARTESIAN_POINT('Ctrl Pts',(-4.28823496303483,-0.999343930726676,
0.533288555311391));
#35794=CARTESIAN_POINT('Ctrl Pts',(-4.21676438031758,-0.989843650280205,
-0.550721820074632));
#35795=CARTESIAN_POINT('Ctrl Pts',(-4.14529379760033,-0.0737523434839011,
-1.1303298487331));
#35796=CARTESIAN_POINT('Ctrl Pts',(-4.07382321488309,0.909888230063614,
-0.674676503146548));
#35797=CARTESIAN_POINT('Ctrl Pts',(-4.00235263216584,1.06016839954784,0.398908435241142));
#35798=CARTESIAN_POINT('Ctrl Pts',(-3.93088204944859,0.239447586020594,
1.1071358672969));
#35799=CARTESIAN_POINT('Ctrl Pts',(-3.85941146673135,-0.80058163313813,
0.801345134001721));
#35800=CARTESIAN_POINT('Ctrl Pts',(-3.7879408840141,-1.10736361243421,-0.238392124372853));
#35801=CARTESIAN_POINT('Ctrl Pts',(-3.71647030129686,-0.399918836166434,
-1.05978766721718));
#35802=CARTESIAN_POINT('Ctrl Pts',(-3.6449997185796,0.673808865727154,-0.910530937186564));
#35803=CARTESIAN_POINT('Ctrl Pts',(-3.57352913586236,1.13039963799526,0.072674847963582));
#35804=CARTESIAN_POINT('Ctrl Pts',(-3.50205855314511,0.551665116510674,
0.989318237136875));
#35805=CARTESIAN_POINT('Ctrl Pts',(-3.43058797042786,-0.532335710452797,
0.999851822263215));
#35806=CARTESIAN_POINT('Ctrl Pts',(-3.35911738771062,-1.12877390268557,
0.0946279648007577));
#35807=CARTESIAN_POINT('Ctrl Pts',(-3.28764680499337,-0.691375801011796,
-0.897264998136924));
#35808=CARTESIAN_POINT('Ctrl Pts',(-3.21617622227613,0.379248666114025,
-1.0673590887593));
#35809=CARTESIAN_POINT('Ctrl Pts',(-3.14470563955887,1.10252187493073,-0.259866293323276));
#35810=CARTESIAN_POINT('Ctrl Pts',(-3.07323505684163,0.816002842433735,
0.785636262049064));
#35811=CARTESIAN_POINT('Ctrl Pts',(-3.00176447412438,-0.217887610001112,
1.11157994067649));
#35812=CARTESIAN_POINT('Ctrl Pts',(-2.93029389140713,-1.05221629131795,
0.419435157552917));
#35813=CARTESIAN_POINT('Ctrl Pts',(-2.85882330868989,-0.922827271139325,
-0.656867416415175));
#35814=CARTESIAN_POINT('Ctrl Pts',(-2.78735272597264,0.051772932289347,
-1.13154961826182));
#35815=CARTESIAN_POINT('Ctrl Pts',(-2.71588214325539,0.978954661287059,
-0.569853267298351));
#35816=CARTESIAN_POINT('Ctrl Pts',(-2.64441156053815,1.00951851444678,0.513767791999302));
#35817=CARTESIAN_POINT('Ctrl Pts',(-2.5729409778209,0.115471267790065,1.12683244602779));
#35818=CARTESIAN_POINT('Ctrl Pts',(-2.50147039510365,-0.884335322929965,
0.707838973018747));
#35819=CARTESIAN_POINT('Ctrl Pts',(-2.4299998123864,-1.07418524238789,-0.359459372036147));
#35820=CARTESIAN_POINT('Ctrl Pts',(-2.35852922966916,-0.280196248383438,
-1.09753133781927));
#35821=CARTESIAN_POINT('Ctrl Pts',(-2.28705864695191,0.770422572284684,
-0.830381861084687));
#35822=CARTESIAN_POINT('Ctrl Pts',(-2.21558806423466,1.11541663057547,0.197308680388403));
#35823=CARTESIAN_POINT('Ctrl Pts',(-2.14411748151742,0.438808229068046,
1.04428555155484));
#35824=CARTESIAN_POINT('Ctrl Pts',(-2.07264689880016,-0.639701626885685,
0.93480843152997));
#35825=CARTESIAN_POINT('Ctrl Pts',(-2.00117631608292,-1.13231313996798,
-0.030853334605713));
#35826=CARTESIAN_POINT('Ctrl Pts',(-1.92970573336567,-0.587846795790038,
-0.968256742613268));
#35827=CARTESIAN_POINT('Ctrl Pts',(-1.85823515064843,0.4950244060751,-1.01884042543795));
#35828=CARTESIAN_POINT('Ctrl Pts',(-1.78676456793118,1.12450614210672,-0.13627513368518));
#35829=CARTESIAN_POINT('Ctrl Pts',(-1.71529398521393,0.724060395961153,
0.871103620044959));
#35830=CARTESIAN_POINT('Ctrl Pts',(-1.64382340249668,-0.339547310642638,
1.08064452961661));
#35831=CARTESIAN_POINT('Ctrl Pts',(-1.57235281977943,-1.09216596230081,
0.300430506912404));
#35832=CARTESIAN_POINT('Ctrl Pts',(-1.50088223706219,-0.844477275441778,
-0.754945757901968));
#35833=CARTESIAN_POINT('Ctrl Pts',(-1.42941165434494,0.176662356954578,
-1.11887237535459));
#35834=CARTESIAN_POINT('Ctrl Pts',(-1.3579410716277,1.03599816963305,-0.458031427443242));
#35835=CARTESIAN_POINT('Ctrl Pts',(-1.28647048891045,0.946470301531875,
0.622317346917095));
#35836=CARTESIAN_POINT('Ctrl Pts',(-1.2149999061932,-0.00992315233657026,
1.13268996675844));
#35837=CARTESIAN_POINT('Ctrl Pts',(-1.14352932347595,-0.957228224473628,
0.60563951031527));
#35838=CARTESIAN_POINT('Ctrl Pts',(-1.07205874075871,-1.02781420127466,
-0.476111866171842));
#35839=CARTESIAN_POINT('Ctrl Pts',(-1.00058815804146,-0.157032780474456,
-1.12179595235208));
#35840=CARTESIAN_POINT('Ctrl Pts',(-0.929117575324211,0.857575021859809,
-0.740034212889895));
#35841=CARTESIAN_POINT('Ctrl Pts',(-0.857646992606967,1.0867335802145,0.31951868111913));
#35842=CARTESIAN_POINT('Ctrl Pts',(-0.786176409889718,0.320564368022132,
1.08642872230062));
#35843=CARTESIAN_POINT('Ctrl Pts',(-0.714705827172471,-0.739215298950436,
0.858282104855236));
#35844=CARTESIAN_POINT('Ctrl Pts',(-0.643235244455224,-1.12193803373525,
-0.15595157858626));
#35845=CARTESIAN_POINT('Ctrl Pts',(-0.571764661737977,-0.477113298122812,
-1.02736478175254));
#35846=CARTESIAN_POINT('Ctrl Pts',(-0.50029407902073,0.604749195542173,
-0.957794082086403));
#35847=CARTESIAN_POINT('Ctrl Pts',(-0.428823496303482,1.1326255269949,-0.0110385894026361));
#35848=CARTESIAN_POINT('Ctrl Pts',(-0.357352913586236,0.623328692801092,
0.945926260653483));
#35849=CARTESIAN_POINT('Ctrl Pts',(-0.285882330868988,-0.457232996199784,
1.03633538397604));
#35850=CARTESIAN_POINT('Ctrl Pts',(-0.214411748151741,-1.11832855125311,
0.177930077439508));
#35851=CARTESIAN_POINT('Ctrl Pts',(-0.142941165434494,-0.756478312243647,
-0.844124685575415));
#35852=CARTESIAN_POINT('Ctrl Pts',(-0.0714705827172459,0.300862454100803,
-1.09171050239691));
#35853=CARTESIAN_POINT('Ctrl Pts',(-0.0238235275724158,0.818068118928352,
-0.592123416550042));
#35854=CARTESIAN_POINT('Ctrl Pts',(0.,0.913908649078056,-0.288121577880454));
#35855=CARTESIAN_POINT('Ctrl Pts',(-7.88382312107629,-0.456179659636056,
0.93887600135061));
#35856=CARTESIAN_POINT('Ctrl Pts',(-7.85999959350388,-0.768486618303383,
0.78713276592667));
#35857=CARTESIAN_POINT('Ctrl Pts',(-7.81235253835904,-1.22437417531279,
0.150151803359993));
#35858=CARTESIAN_POINT('Ctrl Pts',(-7.74088195564181,-0.789007640231457,
-0.949746694351075));
#35859=CARTESIAN_POINT('Ctrl Pts',(-7.66941137292455,0.370030094355424,
-1.17672309148751));
#35860=CARTESIAN_POINT('Ctrl Pts',(-7.5979407902073,1.18963320956613,-0.327482360701716));
#35861=CARTESIAN_POINT('Ctrl Pts',(-7.52647020749006,0.919935306933638,
0.822497367572291));
#35862=CARTESIAN_POINT('Ctrl Pts',(-7.4549996247728,-0.192470224391866,
1.21873687455134));
#35863=CARTESIAN_POINT('Ctrl Pts',(-7.38352904205557,-1.12851713013788,
0.498965038599307));
#35864=CARTESIAN_POINT('Ctrl Pts',(-7.3120584593383,-1.03100320052307,-0.677922102701611));
#35865=CARTESIAN_POINT('Ctrl Pts',(-7.24058787662108,0.0108207282058917,
-1.23384357871844));
#35866=CARTESIAN_POINT('Ctrl Pts',(-7.16911729390382,1.04272284512438,-0.659728538064129));
#35867=CARTESIAN_POINT('Ctrl Pts',(-7.09764671118657,1.11960813357132,0.518644412882883));
#35868=CARTESIAN_POINT('Ctrl Pts',(-7.02617612846932,0.171048889875141,
1.22198550873392));
#35869=CARTESIAN_POINT('Ctrl Pts',(-6.95470554575208,-0.934171226621928,
0.806123172808106));
#35870=CARTESIAN_POINT('Ctrl Pts',(-6.88323496303483,-1.18379117008131,
-0.348064355506461));
#35871=CARTESIAN_POINT('Ctrl Pts',(-6.81176438031758,-0.349184427042679,
-1.1834608081271));
#35872=CARTESIAN_POINT('Ctrl Pts',(-6.74029379760034,0.805237704350161,
-0.934934296665356));
#35873=CARTESIAN_POINT('Ctrl Pts',(-6.66882321488309,1.22214825808638,0.169892504634269));
#35874=CARTESIAN_POINT('Ctrl Pts',(-6.59735263216585,0.519701518345439,
1.1191157312504));
#35875=CARTESIAN_POINT('Ctrl Pts',(-6.52588204944859,-0.658736251058421,
1.04334861833495));
#35876=CARTESIAN_POINT('Ctrl Pts',(-6.45441146673136,-1.23384201389987,
0.0119855915931193));
#35877=CARTESIAN_POINT('Ctrl Pts',(-6.38294088401409,-0.678880308990175,
-1.03035492837643));
#35878=CARTESIAN_POINT('Ctrl Pts',(-6.31147030129687,0.497863220615383,
-1.12900043438899));
#35879=CARTESIAN_POINT('Ctrl Pts',(-6.2399997185796,1.21861723575039,-0.193602159857718));
#35880=CARTESIAN_POINT('Ctrl Pts',(-6.16852913586237,0.823248061552785,
0.919115004067365));
#35881=CARTESIAN_POINT('Ctrl Pts',(-6.09705855314511,-0.326128378451125,
1.1900210269178));
#35882=CARTESIAN_POINT('Ctrl Pts',(-6.02558797042787,-1.17680606853814,
0.370994932716252));
#35883=CARTESIAN_POINT('Ctrl Pts',(-5.95411738771062,-0.949655132463719,
-0.787822881250074));
#35884=CARTESIAN_POINT('Ctrl Pts',(-5.88264680499338,0.147278441370431,
-1.2250791092237));
#35885=CARTESIAN_POINT('Ctrl Pts',(-5.81117622227612,1.10932069855432,-0.540293763417913));
#35886=CARTESIAN_POINT('Ctrl Pts',(-5.73970563955888,1.05534371835782,0.639342943288971));
#35887=CARTESIAN_POINT('Ctrl Pts',(-5.66823505684163,0.0347846476552195,
1.23340982294695));
#35888=CARTESIAN_POINT('Ctrl Pts',(-5.59676447412438,-1.0176334438315,0.697805085271177));
#35889=CARTESIAN_POINT('Ctrl Pts',(-5.52529389140713,-1.1380080272002,-0.476914555304986));
#35890=CARTESIAN_POINT('Ctrl Pts',(-5.45382330868989,-0.216088845205655,
-1.2148314179414));
#35891=CARTESIAN_POINT('Ctrl Pts',(-5.38235272597264,0.903744631539887,
-0.840092497287928));
#35892=CARTESIAN_POINT('Ctrl Pts',(-5.3108821432554,1.19584458407219,0.304081393350546));
#35893=CARTESIAN_POINT('Ctrl Pts',(-5.23941156053815,0.392678664543124,
1.16974921647771));
#35894=CARTESIAN_POINT('Ctrl Pts',(-5.1679409778209,-0.770138956962542,
0.964051736166549));
#35895=CARTESIAN_POINT('Ctrl Pts',(-5.09647039510366,-1.22759157741264,
-0.124614132836987));
#35896=CARTESIAN_POINT('Ctrl Pts',(-5.0249998123864,-0.560701471827329,
-1.0991467702395));
#35897=CARTESIAN_POINT('Ctrl Pts',(-4.95352922966916,0.619731275240731,
-1.06697840162099));
#35898=CARTESIAN_POINT('Ctrl Pts',(-4.88205864695191,1.23255638778736,-0.0575718156892628));
#35899=CARTESIAN_POINT('Ctrl Pts',(-4.81058806423466,0.716491538447744,
1.00456440230082));
#35900=CARTESIAN_POINT('Ctrl Pts',(-4.73911748151742,-0.455803008408689,
1.14662695789119));
#35901=CARTESIAN_POINT('Ctrl Pts',(-4.66764689880017,-1.21063069866651,
0.238501728470574));
#35902=CARTESIAN_POINT('Ctrl Pts',(-4.59617631608292,-0.856650015678725,
-0.888065602123423));
#35903=CARTESIAN_POINT('Ctrl Pts',(-4.52470573336567,0.281930555096303,
-1.20125972426461));
#35904=CARTESIAN_POINT('Ctrl Pts',(-4.45323515064843,1.16229285955041,-0.414228284494605));
#35905=CARTESIAN_POINT('Ctrl Pts',(-4.38176456793118,0.978119086856775,
0.752192006713493));
#35906=CARTESIAN_POINT('Ctrl Pts',(-4.31029398521393,-0.101907264771738,
1.22968478579835));
#35907=CARTESIAN_POINT('Ctrl Pts',(-4.23882340249669,-1.08859744988975,
0.580917683609934));
#35908=CARTESIAN_POINT('Ctrl Pts',(-4.16735281977944,-1.07824867931211,
-0.599907950104766));
#35909=CARTESIAN_POINT('Ctrl Pts',(-4.09588223706219,-0.080339321200062,
-1.23128199715025));
#35910=CARTESIAN_POINT('Ctrl Pts',(-4.02441165434494,0.991152271482454,
-0.734933287974066));
#35911=CARTESIAN_POINT('Ctrl Pts',(-3.95294107162769,1.15485428061016,0.434535790923593));
#35912=CARTESIAN_POINT('Ctrl Pts',(-3.88147048891045,0.2608331561435,1.20601651219767));
#35913=CARTESIAN_POINT('Ctrl Pts',(-3.8099999061932,-0.872083271300817,
0.872914962040671));
#35914=CARTESIAN_POINT('Ctrl Pts',(-3.73852932347595,-1.20626459773467,
-0.259683428984625));
#35915=CARTESIAN_POINT('Ctrl Pts',(-3.66705874075871,-0.435636432891633,
-1.15443954427014));
#35916=CARTESIAN_POINT('Ctrl Pts',(-3.59558815804146,0.733988160022454,
-0.991852380137317));
#35917=CARTESIAN_POINT('Ctrl Pts',(-3.52411757532421,1.23135801943897,0.0791655922768651));
#35918=CARTESIAN_POINT('Ctrl Pts',(-3.45264699260697,0.600935494339756,
1.07767634041016));
#35919=CARTESIAN_POINT('Ctrl Pts',(-3.38117640988972,-0.579879738162589,
1.08915070229317));
#35920=CARTESIAN_POINT('Ctrl Pts',(-3.30970582717247,-1.2295870862718,0.103079388389812));
#35921=CARTESIAN_POINT('Ctrl Pts',(-3.23823524445523,-0.753124035435595,
-0.977401632025656));
#35922=CARTESIAN_POINT('Ctrl Pts',(-3.16676466173798,0.413120166253078,
-1.16268718547691));
#35923=CARTESIAN_POINT('Ctrl Pts',(-3.09529407902073,1.20099043441884,-0.283075501362512));
#35924=CARTESIAN_POINT('Ctrl Pts',(-3.02382349630348,0.888881781400566,
0.855803097523826));
#35925=CARTESIAN_POINT('Ctrl Pts',(-2.95235291358623,-0.237347613085816,
1.21085749516599));
#35926=CARTESIAN_POINT('Ctrl Pts',(-2.88088233086899,-1.14619195278272,
0.456895798200539));
#35927=CARTESIAN_POINT('Ctrl Pts',(-2.80941174815174,-1.00524692567104,
-0.715533634056558));
#35928=CARTESIAN_POINT('Ctrl Pts',(-2.73794116543449,0.056396882325089,
-1.2326107068743));
#35929=CARTESIAN_POINT('Ctrl Pts',(-2.66647058271725,1.06638717169159,-0.620748067325792));
#35930=CARTESIAN_POINT('Ctrl Pts',(-2.595,1.09968074719197,0.559653479657632));
#35931=CARTESIAN_POINT('Ctrl Pts',(-2.52352941728275,0.125784250833858,
1.22747223401548));
#35932=CARTESIAN_POINT('Ctrl Pts',(-2.45205883456551,-0.963317180191378,
0.771057568139225));
#35933=CARTESIAN_POINT('Ctrl Pts',(-2.38058825184826,-1.17012299731723,
-0.391563448484618));
#35934=CARTESIAN_POINT('Ctrl Pts',(-2.30911766913101,-0.30522116768859,
-1.19555418188749));
#35935=CARTESIAN_POINT('Ctrl Pts',(-2.23764708641376,0.839230640963375,
-0.904545020605871));
#35936=CARTESIAN_POINT('Ctrl Pts',(-2.16617650369652,1.21503684795098,0.214930735763543));
#35937=CARTESIAN_POINT('Ctrl Pts',(-2.09470592097927,0.477999119689234,
1.13755290188502));
#35938=CARTESIAN_POINT('Ctrl Pts',(-2.02323533826202,-0.696834731574045,
1.01829814882551));
#35939=CARTESIAN_POINT('Ctrl Pts',(-1.95176475554478,-1.23344242031819,
-0.0336089111462738));
#35940=CARTESIAN_POINT('Ctrl Pts',(-1.88029417282753,-0.640348635887132,
-1.05473379928461));
#35941=CARTESIAN_POINT('Ctrl Pts',(-1.80882359011028,0.539236082311204,
-1.10983521776118));
#35942=CARTESIAN_POINT('Ctrl Pts',(-1.73735300739303,1.22493816297319,-0.148446153973453));
#35943=CARTESIAN_POINT('Ctrl Pts',(-1.66588242467579,0.788727760658277,
0.94890372594861));
#35944=CARTESIAN_POINT('Ctrl Pts',(-1.59441184195854,-0.369872998792028,
1.1771591771439));
#35945=CARTESIAN_POINT('Ctrl Pts',(-1.52294125924129,-1.18970961333854,
0.327262590623961));
#35946=CARTESIAN_POINT('Ctrl Pts',(-1.45147067652405,-0.919899326218264,
-0.822371559568652));
#35947=CARTESIAN_POINT('Ctrl Pts',(-1.3800000938068,0.192440445535514,-1.2188012326021));
#35948=CARTESIAN_POINT('Ctrl Pts',(-1.30852951108955,1.12852535636346,-0.498939182551021));
#35949=CARTESIAN_POINT('Ctrl Pts',(-1.2370589283723,1.0310015650916,0.677897824809409));
#35950=CARTESIAN_POINT('Ctrl Pts',(-1.16558834565506,-0.0108094100502411,
1.23385290230595));
#35951=CARTESIAN_POINT('Ctrl Pts',(-1.09411776293781,-1.04272030087456,
0.659730455362137));
#35952=CARTESIAN_POINT('Ctrl Pts',(-1.02264718022056,-1.1196104604893,-0.518634423486247));
#35953=CARTESIAN_POINT('Ctrl Pts',(-0.951176597503313,-0.171057710081155,
-1.22198592044197));
#35954=CARTESIAN_POINT('Ctrl Pts',(-0.879706014786068,0.934166860058776,
-0.806128232947122));
#35955=CARTESIAN_POINT('Ctrl Pts',(-0.808235432068819,1.18379205372353,
0.348055570023312));
#35956=CARTESIAN_POINT('Ctrl Pts',(-0.736764849351574,0.349194649434331,
1.18345996830485));
#35957=CARTESIAN_POINT('Ctrl Pts',(-0.665294266634325,-0.805236180072444,
0.934937094131386));
#35958=CARTESIAN_POINT('Ctrl Pts',(-0.593823683917079,-1.22214069141385,
-0.169879943766531));
#35959=CARTESIAN_POINT('Ctrl Pts',(-0.522353101199832,-0.519725295441906,
-1.11912090235953));
#35960=CARTESIAN_POINT('Ctrl Pts',(-0.450882518482584,0.658760624694418,
-1.04333669642703));
#35961=CARTESIAN_POINT('Ctrl Pts',(-0.379411935765336,1.2337827072909,-0.0120244691588468));
#35962=CARTESIAN_POINT('Ctrl Pts',(-0.307941353048091,0.678999496132413,
1.03040893477219));
#35963=CARTESIAN_POINT('Ctrl Pts',(-0.236470770330842,-0.498069441725224,
1.12889268803235));
#35964=CARTESIAN_POINT('Ctrl Pts',(-0.165000187613595,-1.21820883842042,
0.193821388817066));
#35965=CARTESIAN_POINT('Ctrl Pts',(-0.0935296048963485,-0.824040989578577,
-0.919515245805508));
#35966=CARTESIAN_POINT('Ctrl Pts',(-0.0220590221791003,0.327733115928909,
-1.18921347534774));
#35967=CARTESIAN_POINT('Ctrl Pts',(0.0255880329657297,0.891131512105092,
-0.645007210688402));
#35968=CARTESIAN_POINT('Ctrl Pts',(0.0494115605381455,0.995531762618636,
-0.313854325117897));
#35969=CARTESIAN_POINT('Ctrl Pts',(-7.83441156053815,-0.493581584468094,
1.01585393951021));
#35970=CARTESIAN_POINT('Ctrl Pts',(-7.81058803296573,-0.831494422630182,
0.851669357863982));
#35971=CARTESIAN_POINT('Ctrl Pts',(-7.76294097782089,-1.32475995513446,
0.162462668923692));
#35972=CARTESIAN_POINT('Ctrl Pts',(-7.69147039510366,-0.85369795210419,
-1.02761591478046));
#35973=CARTESIAN_POINT('Ctrl Pts',(-7.61999981238639,0.400368662685528,
-1.27320198458648));
#35974=CARTESIAN_POINT('Ctrl Pts',(-7.54852922966917,1.28717059629967,-0.354332463243694));
#35975=CARTESIAN_POINT('Ctrl Pts',(-7.47705864695191,0.995360307749618,
0.889933484169499));
#35976=CARTESIAN_POINT('Ctrl Pts',(-7.40558806423466,-0.208250754525212,
1.3186604551169));
#35977=CARTESIAN_POINT('Ctrl Pts',(-7.33411748151742,-1.22104364240448,
0.539874913630573));
#35978=CARTESIAN_POINT('Ctrl Pts',(-7.26264689880017,-1.11553459817094,
-0.733504571125245));
#35979=CARTESIAN_POINT('Ctrl Pts',(-7.19117631608293,0.011707913889056,
-1.33500574983004));
#35980=CARTESIAN_POINT('Ctrl Pts',(-7.11970573336567,1.12821513012698,-0.713819325912764));
#35981=CARTESIAN_POINT('Ctrl Pts',(-7.04823515064843,1.2114042020032,0.561167789222543));
#35982=CARTESIAN_POINT('Ctrl Pts',(-6.97676456793118,0.185073096317893,
1.32217544306809));
#35983=CARTESIAN_POINT('Ctrl Pts',(-6.90529398521393,-1.01076342283306,
0.872216777987256));
#35984=CARTESIAN_POINT('Ctrl Pts',(-6.83382340249668,-1.28084957114099,
-0.376601964727679));
#35985=CARTESIAN_POINT('Ctrl Pts',(-6.76235281977945,-0.377813870326487,
-1.28049212298791));
#35986=CARTESIAN_POINT('Ctrl Pts',(-6.69088223706219,0.871258710446879,
-1.01158905657877));
#35987=CARTESIAN_POINT('Ctrl Pts',(-6.61941165434495,1.32235153615238,0.183821899673327));
#35988=CARTESIAN_POINT('Ctrl Pts',(-6.54794107162769,0.562311566193189,
1.21087142788093));
#35989=CARTESIAN_POINT('Ctrl Pts',(-6.47647048891046,-0.712745681829367,
1.12889221014639));
#35990=CARTESIAN_POINT('Ctrl Pts',(-6.40499990619319,-1.33500405671283,
0.0129682837986347));
#35991=CARTESIAN_POINT('Ctrl Pts',(-6.33352932347597,-0.734541340231837,
-1.11483317453981));
#35992=CARTESIAN_POINT('Ctrl Pts',(-6.26205874075869,0.538682758182991,
-1.2215665725111));
#35993=CARTESIAN_POINT('Ctrl Pts',(-6.19058815804147,1.31853100719504,-0.209475496770861));
#35994=CARTESIAN_POINT('Ctrl Pts',(-6.11911757532421,0.890745727145539,
0.994472748692709));
#35995=CARTESIAN_POINT('Ctrl Pts',(-6.04764699260697,-0.352867468716904,
1.28759021058733));
#35996=CARTESIAN_POINT('Ctrl Pts',(-5.97617640988972,-1.27329176488084,
0.401412607624421));
#35997=CARTESIAN_POINT('Ctrl Pts',(-5.90470582717247,-1.02751684578324,
-0.852416055371398));
#35998=CARTESIAN_POINT('Ctrl Pts',(-5.83323524445523,0.159353721530679,
-1.32552268619742));
#35999=CARTESIAN_POINT('Ctrl Pts',(-5.76176466173798,1.20027330572462,-0.584592158358864));
#36000=CARTESIAN_POINT('Ctrl Pts',(-5.69029407902073,1.1418707819658,0.691762327191066));
#36001=CARTESIAN_POINT('Ctrl Pts',(-5.61882349630349,0.0376366221995333,
1.33453643065623));
#36002=CARTESIAN_POINT('Ctrl Pts',(-5.54735291358624,-1.10106866232222,
0.755017748737059));
#36003=CARTESIAN_POINT('Ctrl Pts',(-5.47588233086899,-1.23131269301009,
-0.51601652307587));
#36004=CARTESIAN_POINT('Ctrl Pts',(-5.40441174815174,-0.233805853350823,
-1.31443479222096));
#36005=CARTESIAN_POINT('Ctrl Pts',(-5.33294116543449,0.977842167592207,
-0.908971229102938));
#36006=CARTESIAN_POINT('Ctrl Pts',(-5.26147058271725,1.29389123805927,0.329012863170987));
#36007=CARTESIAN_POINT('Ctrl Pts',(-5.19,0.42487417695618,1.26565632531713));
#36008=CARTESIAN_POINT('Ctrl Pts',(-5.11852941728275,-0.833282235646911,
1.04309381927713));
#36009=CARTESIAN_POINT('Ctrl Pts',(-5.04705883456551,-1.32824115030125,
-0.134831178535808));
#36010=CARTESIAN_POINT('Ctrl Pts',(-4.97558825184826,-0.606673083799771,
-1.18926522250167));
#36011=CARTESIAN_POINT('Ctrl Pts',(-4.90411766913101,0.670542709032212,
-1.15445938664932));
#36012=CARTESIAN_POINT('Ctrl Pts',(-4.83264708641377,1.33361302280713,-0.0622920978793508));
#36013=CARTESIAN_POINT('Ctrl Pts',(-4.76117650369652,0.77523629415475,1.08692809710864));
#36014=CARTESIAN_POINT('Ctrl Pts',(-4.68970592097927,-0.493174051809261,
1.24063828519075));
#36015=CARTESIAN_POINT('Ctrl Pts',(-4.61823533826202,-1.30988965823305,
0.25805635685469));
#36016=CARTESIAN_POINT('Ctrl Pts',(-4.54676475554478,-0.926886289517314,
-0.960877622990471));
#36017=CARTESIAN_POINT('Ctrl Pts',(-4.47529417282753,0.30504588960722,-1.29975036268229));
#36018=CARTESIAN_POINT('Ctrl Pts',(-4.40382359011029,1.25758862569748,-0.448190638652046));
#36019=CARTESIAN_POINT('Ctrl Pts',(-4.33235300739303,1.05831454448108,0.81386382460385));
#36020=CARTESIAN_POINT('Ctrl Pts',(-4.26088242467579,-0.110262586576019,
1.3305059797162));
#36021=CARTESIAN_POINT('Ctrl Pts',(-4.18941184195854,-1.17785096905283,
0.628546811908475));
#36022=CARTESIAN_POINT('Ctrl Pts',(-4.11794125924129,-1.16665370834401,
-0.649094080134899));
#36023=CARTESIAN_POINT('Ctrl Pts',(-4.04647067652405,-0.0869262989162214,
-1.33223414556741));
#36024=CARTESIAN_POINT('Ctrl Pts',(-3.9750000938068,1.07241631290129,-0.795190072801583));
#36025=CARTESIAN_POINT('Ctrl Pts',(-3.90352951108955,1.24954016167249,0.470163146606043));
#36026=CARTESIAN_POINT('Ctrl Pts',(-3.83205892837231,0.282218726266407,
1.30489715709843));
#36027=CARTESIAN_POINT('Ctrl Pts',(-3.76058834565505,-0.943584909463504,
0.94448479007962));
#36028=CARTESIAN_POINT('Ctrl Pts',(-3.68911776293781,-1.30516558303513,
-0.280974733596397));
#36029=CARTESIAN_POINT('Ctrl Pts',(-3.61764718022056,-0.471354029616834,
-1.24909142132311));
#36030=CARTESIAN_POINT('Ctrl Pts',(-3.54617659750332,0.794167454317755,
-1.07317382308807));
#36031=CARTESIAN_POINT('Ctrl Pts',(-3.47470601478607,1.33231640088267,0.0856563365901476));
#36032=CARTESIAN_POINT('Ctrl Pts',(-3.40323543206882,0.650205872168837,
1.16603444368344));
#36033=CARTESIAN_POINT('Ctrl Pts',(-3.33176484935158,-0.627423765872378,
1.17844958232312));
#36034=CARTESIAN_POINT('Ctrl Pts',(-3.26029426663432,-1.33040026985804,
0.111530811978866));
#36035=CARTESIAN_POINT('Ctrl Pts',(-3.18882368391708,-0.814872269859391,
-1.05753826591439));
#36036=CARTESIAN_POINT('Ctrl Pts',(-3.11735310119983,0.44699166639213,-1.25801528219453));
#36037=CARTESIAN_POINT('Ctrl Pts',(-3.04588251848259,1.29945899390695,-0.306284709401745));
#36038=CARTESIAN_POINT('Ctrl Pts',(-2.97441193576534,0.961760720367394,
0.925969932998585));
#36039=CARTESIAN_POINT('Ctrl Pts',(-2.90294135304809,-0.256807616170518,
1.3101350496555));
#36040=CARTESIAN_POINT('Ctrl Pts',(-2.83147077033084,-1.2401676142475,0.49435643884816));
#36041=CARTESIAN_POINT('Ctrl Pts',(-2.7600001876136,-1.08766658020275,-0.77419985169794));
#36042=CARTESIAN_POINT('Ctrl Pts',(-2.68852960489635,0.061020832360832,
-1.33367179548678));
#36043=CARTESIAN_POINT('Ctrl Pts',(-2.6170590221791,1.15381968209612,-0.671642867353233));
#36044=CARTESIAN_POINT('Ctrl Pts',(-2.54558843946185,1.18984297993716,0.605539167315962));
#36045=CARTESIAN_POINT('Ctrl Pts',(-2.47411785674461,0.136097233877648,
1.32811202200318));
#36046=CARTESIAN_POINT('Ctrl Pts',(-2.40264727402736,-1.04229903745279,
0.834276163259703));
#36047=CARTESIAN_POINT('Ctrl Pts',(-2.33117669131011,-1.26606075224656,
-0.423667524933089));
#36048=CARTESIAN_POINT('Ctrl Pts',(-2.25970610859287,-0.330246086993743,
-1.2935770259557));
#36049=CARTESIAN_POINT('Ctrl Pts',(-2.18823552587562,0.908038709642064,
-0.978708180127054));
#36050=CARTESIAN_POINT('Ctrl Pts',(-2.11676494315837,1.3146570653265,0.232552791138683));
#36051=CARTESIAN_POINT('Ctrl Pts',(-2.04529436044112,0.517190010310421,
1.2308202522152));
#36052=CARTESIAN_POINT('Ctrl Pts',(-1.97382377772388,-0.753967836262407,
1.10178786612104));
#36053=CARTESIAN_POINT('Ctrl Pts',(-1.90235319500663,-1.3345717006684,-0.0363644876868344));
#36054=CARTESIAN_POINT('Ctrl Pts',(-1.83088261228938,-0.692850475984229,
-1.14121085595595));
#36055=CARTESIAN_POINT('Ctrl Pts',(-1.75941202957214,0.583447758547311,
-1.20083001008441));
#36056=CARTESIAN_POINT('Ctrl Pts',(-1.68794144685489,1.32537018383966,-0.160617174261725));
#36057=CARTESIAN_POINT('Ctrl Pts',(-1.61647086413764,0.853395125355401,
1.02670383185226));
#36058=CARTESIAN_POINT('Ctrl Pts',(-1.54500028142039,-0.400198686941418,
1.27367382467119));
#36059=CARTESIAN_POINT('Ctrl Pts',(-1.47352969870315,-1.28725326437627,
0.354094674335519));
#36060=CARTESIAN_POINT('Ctrl Pts',(-1.4020591159859,-0.995321376994749,
-0.889797361235337));
#36061=CARTESIAN_POINT('Ctrl Pts',(-1.33058853326865,0.20821853411645,-1.31873008984962));
#36062=CARTESIAN_POINT('Ctrl Pts',(-1.2591179505514,1.22105254309388,-0.539846937658801));
#36063=CARTESIAN_POINT('Ctrl Pts',(-1.18764736783416,1.11553282865133,0.733478302701723));
#36064=CARTESIAN_POINT('Ctrl Pts',(-1.11617678511691,-0.0116956677639116,
1.33501583785347));
#36065=CARTESIAN_POINT('Ctrl Pts',(-1.04470620239966,-1.12821237727549,
0.713821400409003));
#36066=CARTESIAN_POINT('Ctrl Pts',(-0.973235619682415,-1.21140671970395,
-0.561156980800651));
#36067=CARTESIAN_POINT('Ctrl Pts',(-0.90176503696517,-0.185082639687852,
-1.32217588853185));
#36068=CARTESIAN_POINT('Ctrl Pts',(-0.830294454247922,1.01075869825774,
-0.872222253004347));
#36069=CARTESIAN_POINT('Ctrl Pts',(-0.758823871530675,1.28085052723256,
0.376592458927494));
#36070=CARTESIAN_POINT('Ctrl Pts',(-0.687353288813427,0.37782493084653,
1.28049121430909));
#36071=CARTESIAN_POINT('Ctrl Pts',(-0.61588270609618,-0.871257061194453,
1.01159208340753));
#36072=CARTESIAN_POINT('Ctrl Pts',(-0.544412123378933,-1.32234334909244,
-0.1838083089468));
#36073=CARTESIAN_POINT('Ctrl Pts',(-0.472941540661686,-0.562337292761001,
-1.21087702296652));
#36074=CARTESIAN_POINT('Ctrl Pts',(-0.401470957944439,0.712772053846664,
-1.12887931076765));
#36075=CARTESIAN_POINT('Ctrl Pts',(-0.330000375227191,1.33493988758691,
-0.0130103489150566));
#36076=CARTESIAN_POINT('Ctrl Pts',(-0.258529792509945,0.734670299463734,
1.1148916088909));
#36077=CARTESIAN_POINT('Ctrl Pts',(-0.187059209792697,-0.538905887250664,
1.22144999208865));
#36078=CARTESIAN_POINT('Ctrl Pts',(-0.11558862707545,-1.31808912558773,
0.209712700194622));
#36079=CARTESIAN_POINT('Ctrl Pts',(-0.044118044358203,-0.891603666913505,
-0.994905806035601));
#36080=CARTESIAN_POINT('Ctrl Pts',(0.0273525383590451,0.354603777757012,
-1.28671644829858));
#36081=CARTESIAN_POINT('Ctrl Pts',(0.0749995935038751,0.964194905281832,
-0.697891004826763));
#36082=CARTESIAN_POINT('Ctrl Pts',(0.0988231210762909,1.07715487615921,
-0.33958707235534));
#36083=CARTESIAN_POINT('Ctrl Pts',(-7.785,-0.530983509300131,1.09283187766981));
#36084=CARTESIAN_POINT('Ctrl Pts',(-7.76117647242759,-0.89450222695698,
0.916205949801296));
#36085=CARTESIAN_POINT('Ctrl Pts',(-7.71352941728276,-1.42514573495613,
0.174773534487387));
#36086=CARTESIAN_POINT('Ctrl Pts',(-7.6420588345655,-0.918388263976919,
-1.10548513520984));
#36087=CARTESIAN_POINT('Ctrl Pts',(-7.57058825184826,0.43070723101563,-1.36968087768545));
#36088=CARTESIAN_POINT('Ctrl Pts',(-7.499117669131,1.38470798303322,-0.381182565785671));
#36089=CARTESIAN_POINT('Ctrl Pts',(-7.42764708641377,1.0707853085656,0.957369600766706));
#36090=CARTESIAN_POINT('Ctrl Pts',(-7.35617650369651,-0.224031284658557,
1.41858403568246));
#36091=CARTESIAN_POINT('Ctrl Pts',(-7.28470592097928,-1.31357015467109,
0.580784788661838));
#36092=CARTESIAN_POINT('Ctrl Pts',(-7.21323533826202,-1.20006599581882,
-0.789087039548876));
#36093=CARTESIAN_POINT('Ctrl Pts',(-7.14176475554478,0.0125950995722171,
-1.43616792094163));
#36094=CARTESIAN_POINT('Ctrl Pts',(-7.07029417282752,1.21370741512959,-0.767910113761398));
#36095=CARTESIAN_POINT('Ctrl Pts',(-6.99882359011029,1.30320027043509,0.603691165562203));
#36096=CARTESIAN_POINT('Ctrl Pts',(-6.92735300739303,0.199097302760646,
1.42236537740225));
#36097=CARTESIAN_POINT('Ctrl Pts',(-6.85588242467579,-1.08735561904419,
0.938310383166409));
#36098=CARTESIAN_POINT('Ctrl Pts',(-6.78441184195853,-1.37790797220067,
-0.405139573948898));
#36099=CARTESIAN_POINT('Ctrl Pts',(-6.7129412592413,-0.406443313610296,
-1.37752343784872));
#36100=CARTESIAN_POINT('Ctrl Pts',(-6.64147067652404,0.937279716543598,
-1.08824381649219));
#36101=CARTESIAN_POINT('Ctrl Pts',(-6.5700000938068,1.42255481421838,0.197751294712385));
#36102=CARTESIAN_POINT('Ctrl Pts',(-6.49852951108955,0.604921614040939,
1.30262712451147));
#36103=CARTESIAN_POINT('Ctrl Pts',(-6.4270589283723,-0.766755112600313,
1.21443580195783));
#36104=CARTESIAN_POINT('Ctrl Pts',(-6.35558834565506,-1.43616609952579,
0.0139509760041505));
#36105=CARTESIAN_POINT('Ctrl Pts',(-6.28411776293781,-0.790202371473498,
-1.19931142070319));
#36106=CARTESIAN_POINT('Ctrl Pts',(-6.21264718022056,0.579502295750599,
-1.31413271063321));
#36107=CARTESIAN_POINT('Ctrl Pts',(-6.14117659750332,1.41844477863968,-0.225348833684005));
#36108=CARTESIAN_POINT('Ctrl Pts',(-6.06970601478607,0.958243392738293,
1.06983049331806));
#36109=CARTESIAN_POINT('Ctrl Pts',(-5.99823543206882,-0.379606558982684,
1.38515939425687));
#36110=CARTESIAN_POINT('Ctrl Pts',(-5.92676484935158,-1.36977746122354,
0.431830282532593));
#36111=CARTESIAN_POINT('Ctrl Pts',(-5.85529426663433,-1.10537855910276,
-0.917009229492723));
#36112=CARTESIAN_POINT('Ctrl Pts',(-5.78382368391709,0.171429001690927,
-1.42596626317113));
#36113=CARTESIAN_POINT('Ctrl Pts',(-5.71235310119983,1.29122591289492,-0.628890553299815));
#36114=CARTESIAN_POINT('Ctrl Pts',(-5.64088251848259,1.22839784557378,0.74418171109316));
#36115=CARTESIAN_POINT('Ctrl Pts',(-5.56941193576534,0.0404885967438472,
1.43566303836552));
#36116=CARTESIAN_POINT('Ctrl Pts',(-5.49794135304809,-1.18450388081295,
0.81223041220294));
#36117=CARTESIAN_POINT('Ctrl Pts',(-5.42647077033085,-1.32461735881998,
-0.555118490846752));
#36118=CARTESIAN_POINT('Ctrl Pts',(-5.3550001876136,-0.251522861495992,
-1.41403816650052));
#36119=CARTESIAN_POINT('Ctrl Pts',(-5.28352960489635,1.05193970364453,-0.977849960917949));
#36120=CARTESIAN_POINT('Ctrl Pts',(-5.2120590221791,1.39193789204635,0.353944332991429));
#36121=CARTESIAN_POINT('Ctrl Pts',(-5.14058843946187,0.457069689369236,
1.36156343415655));
#36122=CARTESIAN_POINT('Ctrl Pts',(-5.0691178567446,-0.896425514331279,
1.12213590238771));
#36123=CARTESIAN_POINT('Ctrl Pts',(-4.99764727402737,-1.42889072318987,
-0.145048224234627));
#36124=CARTESIAN_POINT('Ctrl Pts',(-4.92617669131011,-0.652644695772212,
-1.27938367476384));
#36125=CARTESIAN_POINT('Ctrl Pts',(-4.85470610859287,0.721354142823692,
-1.24194037167764));
#36126=CARTESIAN_POINT('Ctrl Pts',(-4.78323552587561,1.4346696578269,-0.0670123800694382));
#36127=CARTESIAN_POINT('Ctrl Pts',(-4.71176494315838,0.833981049861757,
1.16929179191647));
#36128=CARTESIAN_POINT('Ctrl Pts',(-4.64029436044112,-0.530545095209834,
1.33464961249031));
#36129=CARTESIAN_POINT('Ctrl Pts',(-4.56882377772388,-1.40914861779958,
0.277610985238807));
#36130=CARTESIAN_POINT('Ctrl Pts',(-4.49735319500663,-0.997122563355904,
-1.03368964385752));
#36131=CARTESIAN_POINT('Ctrl Pts',(-4.42588261228939,0.328161224118138,
-1.39824100109996));
#36132=CARTESIAN_POINT('Ctrl Pts',(-4.35441202957214,1.35288439184455,-0.482152992809488));
#36133=CARTESIAN_POINT('Ctrl Pts',(-4.28294144685489,1.13851000210538,0.875535642494211));
#36134=CARTESIAN_POINT('Ctrl Pts',(-4.21147086413764,-0.118617908380299,
1.43132717363404));
#36135=CARTESIAN_POINT('Ctrl Pts',(-4.14000028142039,-1.26710448821591,
0.676175940207019));
#36136=CARTESIAN_POINT('Ctrl Pts',(-4.06852969870315,-1.25505873737591,
-0.698280210165035));
#36137=CARTESIAN_POINT('Ctrl Pts',(-3.9970591159859,-0.0935132766323821,
-1.43318629398456));
#36138=CARTESIAN_POINT('Ctrl Pts',(-3.92558853326866,1.15368035432013,-0.855446857629104));
#36139=CARTESIAN_POINT('Ctrl Pts',(-3.8541179505514,1.34422604273481,0.505790502288495));
#36140=CARTESIAN_POINT('Ctrl Pts',(-3.78264736783416,0.303604296389314,
1.4037778019992));
#36141=CARTESIAN_POINT('Ctrl Pts',(-3.71117678511691,-1.01508654762619,
1.01605461811857));
#36142=CARTESIAN_POINT('Ctrl Pts',(-3.63970620239967,-1.40406656833559,
-0.302266038208169));
#36143=CARTESIAN_POINT('Ctrl Pts',(-3.56823561968241,-0.507071626342034,
-1.34374329837606));
#36144=CARTESIAN_POINT('Ctrl Pts',(-3.49676503696517,0.854346748613055,
-1.15449526603882));
#36145=CARTESIAN_POINT('Ctrl Pts',(-3.42529445424792,1.43327478232637,0.0921470809034307));
#36146=CARTESIAN_POINT('Ctrl Pts',(-3.35382387153068,0.699476249997918,
1.25439254695673));
#36147=CARTESIAN_POINT('Ctrl Pts',(-3.28235328881343,-0.67496779358217,
1.26774846235307));
#36148=CARTESIAN_POINT('Ctrl Pts',(-3.21088270609618,-1.43121345344427,
0.119982235567921));
#36149=CARTESIAN_POINT('Ctrl Pts',(-3.13941212337893,-0.87662050428319,
-1.13767489980312));
#36150=CARTESIAN_POINT('Ctrl Pts',(-3.06794154066169,0.480863166531182,
-1.35334337891214));
#36151=CARTESIAN_POINT('Ctrl Pts',(-2.99647095794444,1.39792755339507,-0.32949391744098));
#36152=CARTESIAN_POINT('Ctrl Pts',(-2.9250003752272,1.03463965933422,0.996136768473347));
#36153=CARTESIAN_POINT('Ctrl Pts',(-2.85352979250994,-0.276267619255219,
1.409412604145));
#36154=CARTESIAN_POINT('Ctrl Pts',(-2.7820592097927,-1.33414327571228,0.531817079495782));
#36155=CARTESIAN_POINT('Ctrl Pts',(-2.71058862707545,-1.17008623473447,
-0.832866069339323));
#36156=CARTESIAN_POINT('Ctrl Pts',(-2.63911804435821,0.0656447823965748,
-1.43473288409926));
#36157=CARTESIAN_POINT('Ctrl Pts',(-2.56764746164095,1.24125219250066,-0.722537667380674));
#36158=CARTESIAN_POINT('Ctrl Pts',(-2.49617687892371,1.28000521268235,0.651424854974292));
#36159=CARTESIAN_POINT('Ctrl Pts',(-2.42470629620646,0.146410216921439,
1.42875180999087));
#36160=CARTESIAN_POINT('Ctrl Pts',(-2.35323571348922,-1.1212808947142,0.897494758380182));
#36161=CARTESIAN_POINT('Ctrl Pts',(-2.28176513077196,-1.3619985071759,-0.455771601381561));
#36162=CARTESIAN_POINT('Ctrl Pts',(-2.21029454805472,-0.355271006298895,
-1.39159987002391));
#36163=CARTESIAN_POINT('Ctrl Pts',(-2.13882396533747,0.976846778320755,
-1.05287133964824));
#36164=CARTESIAN_POINT('Ctrl Pts',(-2.06735338262022,1.41427728270201,0.250174846513822));
#36165=CARTESIAN_POINT('Ctrl Pts',(-1.99588279990298,0.556380900931609,
1.32408760254539));
#36166=CARTESIAN_POINT('Ctrl Pts',(-1.92441221718573,-0.811100940950769,
1.18527758341658));
#36167=CARTESIAN_POINT('Ctrl Pts',(-1.85294163446849,-1.43570098101862,
-0.0391200642273951));
#36168=CARTESIAN_POINT('Ctrl Pts',(-1.78147105175124,-0.745352316081325,
-1.22768791262729));
#36169=CARTESIAN_POINT('Ctrl Pts',(-1.71000046903399,0.627659434783417,
-1.29182480240764));
#36170=CARTESIAN_POINT('Ctrl Pts',(-1.63852988631674,1.42580220470614,-0.172788194549996));
#36171=CARTESIAN_POINT('Ctrl Pts',(-1.5670593035995,0.918062490052525,1.10450393775591));
#36172=CARTESIAN_POINT('Ctrl Pts',(-1.49558872088225,-0.430524375090808,
1.37018847219848));
#36173=CARTESIAN_POINT('Ctrl Pts',(-1.424118138165,-1.38479691541401,0.380926758047075));
#36174=CARTESIAN_POINT('Ctrl Pts',(-1.35264755544775,-1.07074342777124,
-0.957223162902021));
#36175=CARTESIAN_POINT('Ctrl Pts',(-1.28117697273051,0.223996622697387,
-1.41865894709713));
#36176=CARTESIAN_POINT('Ctrl Pts',(-1.20970639001326,1.3135797298243,-0.58075469276658));
#36177=CARTESIAN_POINT('Ctrl Pts',(-1.13823580729601,1.20006409221106,0.789058780594037));
#36178=CARTESIAN_POINT('Ctrl Pts',(-1.06676522457877,-0.0125819254775816,
1.43617877340099));
#36179=CARTESIAN_POINT('Ctrl Pts',(-0.995294641861518,-1.21370445367643,
0.767912345455868));
#36180=CARTESIAN_POINT('Ctrl Pts',(-0.92382405914427,-1.30320297891858,
-0.603679538115054));
#36181=CARTESIAN_POINT('Ctrl Pts',(-0.852353476427024,-0.199107569294552,
-1.42236585662174));
#36182=CARTESIAN_POINT('Ctrl Pts',(-0.780882893709775,1.08735053645671,
-0.938316273061573));
#36183=CARTESIAN_POINT('Ctrl Pts',(-0.70941231099253,1.37790900074158,0.405129347831677));
#36184=CARTESIAN_POINT('Ctrl Pts',(-0.637941728275282,0.406455212258731,
1.37752246031332));
#36185=CARTESIAN_POINT('Ctrl Pts',(-0.566471145558034,-0.937277942316462,
1.08824707268368));
#36186=CARTESIAN_POINT('Ctrl Pts',(-0.495000562840789,-1.42254600677103,
-0.197736674127072));
#36187=CARTESIAN_POINT('Ctrl Pts',(-0.42352998012354,-0.604949290080097,
-1.30263314357351));
#36188=CARTESIAN_POINT('Ctrl Pts',(-0.352059397406293,0.766783482998911,
-1.21442192510827));
#36189=CARTESIAN_POINT('Ctrl Pts',(-0.280588814689045,1.43609706788291,
-0.0139962286712674));
#36190=CARTESIAN_POINT('Ctrl Pts',(-0.209118231971799,0.790341102795055,
1.19937428300961));
#36191=CARTESIAN_POINT('Ctrl Pts',(-0.137647649254551,-0.579742332776104,
1.31400729614496));
#36192=CARTESIAN_POINT('Ctrl Pts',(-0.0661770665373043,-1.41796941275505,
0.22560401157218));
#36193=CARTESIAN_POINT('Ctrl Pts',(0.00529351617994245,-0.959166344248434,
-1.0702963662657));
#36194=CARTESIAN_POINT('Ctrl Pts',(0.0767640988971906,0.381474439585117,
-1.38421942124942));
#36195=CARTESIAN_POINT('Ctrl Pts',(0.124411154042021,1.03725829845857,-0.750774798965123));
#36196=CARTESIAN_POINT('Ctrl Pts',(0.148234681614436,1.15877798969979,-0.365319819592783));
#36197=CARTESIAN_POINT('',(3.3695633096113E-15,-0.876371264439109,-0.844383392149627));
#36198=CARTESIAN_POINT('Ctrl Pts',(-1.66533453693773E-16,-0.876385019502678,
-0.844404278593171));
#36199=CARTESIAN_POINT('Ctrl Pts',(-1.66201775279586E-16,-0.853668716120764,
-0.863815852990219));
#36200=CARTESIAN_POINT('Ctrl Pts',(-4.86302334741944E-16,-0.830222915225709,
-0.882299336152847));
#36201=CARTESIAN_POINT('Ctrl Pts',(-3.33066907387547E-16,-0.806064413927853,
-0.899791837105119));
#36202=CARTESIAN_POINT('Ctrl Pts',(-8.90510441733197E-17,-0.767426558861498,
-0.927768436655273));
#36203=CARTESIAN_POINT('Ctrl Pts',(-1.71711545508733E-15,-0.726965954730414,
-0.953212246495642));
#36204=CARTESIAN_POINT('Ctrl Pts',(-1.80411241501588E-15,-0.684965814764286,
-0.976084216881709));
#36205=CARTESIAN_POINT('Ctrl Pts',(-1.85091247889602E-15,-0.662371815675076,
-0.988388206308602));
#36206=CARTESIAN_POINT('Ctrl Pts',(8.90055551083889E-16,-0.639332066021806,
-0.999947230709396));
#36207=CARTESIAN_POINT('Ctrl Pts',(1.0547118733939E-15,-0.615890017093324,
-1.01075029848142));
#36208=CARTESIAN_POINT('Ctrl Pts',(1.12586562016508E-15,-0.605759889140421,
-1.01541868131554));
#36209=CARTESIAN_POINT('Ctrl Pts',(1.07131306105525E-15,-0.595554774413637,
-1.01994564355146));
#36210=CARTESIAN_POINT('Ctrl Pts',(9.15933995315754E-16,-0.585291173178408,
-1.02432501098259));
#36211=CARTESIAN_POINT('Ctrl Pts',(2.2127133981659E-16,-0.539405065837525,
-1.04390411576504));
#36212=CARTESIAN_POINT('Ctrl Pts',(-1.96359358092282E-15,-0.49228587059037,
-1.06056774636267));
#36213=CARTESIAN_POINT('Ctrl Pts',(-2.95596880306448E-15,-0.44425982933865,
-1.07426808122273));
#36214=CARTESIAN_POINT('Ctrl Pts',(-3.57545733071877E-15,-0.414279655589566,
-1.08282049172379));
#36215=CARTESIAN_POINT('Ctrl Pts',(-9.63093987522759E-16,-0.383945872099603,
-1.09021711713024));
#36216=CARTESIAN_POINT('Ctrl Pts',(-8.74300631892311E-16,-0.353338310232677,
-1.09643602014208));
#36217=CARTESIAN_POINT('Ctrl Pts',(-8.32779690395146E-16,-0.33902581154824,
-1.09934406102304));
#36218=CARTESIAN_POINT('Ctrl Pts',(-4.61009343396251E-16,-0.324653469259868,
-1.1019944657249));
#36219=CARTESIAN_POINT('Ctrl Pts',(-3.33066907387547E-16,-0.310229613717086,
-1.10438439507686));
#36220=CARTESIAN_POINT('Ctrl Pts',(-2.47338154619976E-16,-0.300564805195711,
-1.10598578449024));
#36221=CARTESIAN_POINT('Ctrl Pts',(-1.61299260203782E-15,-0.290881931078401,
-1.10746931579312));
#36222=CARTESIAN_POINT('Ctrl Pts',(-1.63757896132211E-15,-0.281191356984365,
-1.108833510341));
#36223=CARTESIAN_POINT('Ctrl Pts',(-1.7595790972034E-15,-0.233105695233064,
-1.11560278912219));
#36224=CARTESIAN_POINT('Ctrl Pts',(-1.19024471319125E-15,-0.184770819851817,
-1.11944780780858));
#36225=CARTESIAN_POINT('Ctrl Pts',(-1.20736753927986E-15,-0.136487869923575,
-1.1203187821722));
#36226=CARTESIAN_POINT('Ctrl Pts',(-1.2240112256568E-15,-0.0895559982920508,
-1.12116538448396));
#36227=CARTESIAN_POINT('Ctrl Pts',(-2.22001881418049E-15,-0.0426721509549466,
-1.11920180597511));
#36228=CARTESIAN_POINT('Ctrl Pts',(-2.08166817117217E-15,0.0038740908008012,
-1.11433562929591));
#36229=CARTESIAN_POINT('Ctrl Pts',(-2.00950571302812E-15,0.0281521942445265,
-1.11179747505753));
#36230=CARTESIAN_POINT('Ctrl Pts',(-7.50224596214795E-16,0.0523381381697833,
-1.1084688905888));
#36231=CARTESIAN_POINT('Ctrl Pts',(-1.11022302462516E-15,0.0763879906706078,
-1.10433182603949));
#36232=CARTESIAN_POINT('Ctrl Pts',(-1.32231052695403E-15,0.0905565890469971,
-1.10189453849045));
#36233=CARTESIAN_POINT('Ctrl Pts',(1.23352088475356E-15,0.10467791009547,
-1.09917658032639));
#36234=CARTESIAN_POINT('Ctrl Pts',(1.40165656858926E-15,0.118742544221765,
-1.09617371376713));
#36235=CARTESIAN_POINT('Ctrl Pts',(1.5055427343467E-15,0.127432673995702,
-1.09431832955596));
#36236=CARTESIAN_POINT('Ctrl Pts',(-2.67693673802542E-16,0.136100883638701,
-1.09235410866341));
#36237=CARTESIAN_POINT('Ctrl Pts',(-3.33066907387547E-16,0.144731539974336,
-1.09028355436426));
#36238=CARTESIAN_POINT('Ctrl Pts',(-6.67218484523858E-16,0.188846650519144,
-1.07970003345418));
#36239=CARTESIAN_POINT('Ctrl Pts',(-3.27749510057336E-15,0.232073502898363,
-1.0663233603394));
#36240=CARTESIAN_POINT('Ctrl Pts',(-2.98372437868011E-15,0.274146266817965,
-1.05007992390509));
#36241=CARTESIAN_POINT('Ctrl Pts',(-2.95431841155954E-15,0.278357681435861,
-1.04845398257699));
#36242=CARTESIAN_POINT('Ctrl Pts',(-9.03487711860832E-16,0.282557511928685,
-1.0467992790516));
#36243=CARTESIAN_POINT('Ctrl Pts',(-8.88178419700125E-16,0.286745476895236,
-1.04511571412866));
#36244=CARTESIAN_POINT('Ctrl Pts',(-7.16151853340391E-16,0.3264740599549,
-1.02914479521899));
#36245=CARTESIAN_POINT('Ctrl Pts',(-2.16871884646574E-15,0.365137127092165,
-1.01057884773605));
#36246=CARTESIAN_POINT('Ctrl Pts',(-2.4980018054066E-15,0.402568927230115,
-0.989600059824713));
#36247=CARTESIAN_POINT('Ctrl Pts',(-2.66197985924992E-15,0.421209411263105,
-0.97915293305946));
#36248=CARTESIAN_POINT('Ctrl Pts',(-1.4513023456678E-15,0.439544124644693,
-0.968107023694203));
#36249=CARTESIAN_POINT('Ctrl Pts',(-1.49880108324396E-15,0.457549730619664,
-0.956482776639175));
#36250=CARTESIAN_POINT('Ctrl Pts',(-1.53878850873768E-15,0.472707982483494,
-0.946696754173037));
#36251=CARTESIAN_POINT('Ctrl Pts',(-4.68193304594181E-16,0.487632955649028,
-0.936500815894636));
#36252=CARTESIAN_POINT('Ctrl Pts',(-6.52256026967279E-16,0.502309521134179,
-0.925906648036467));
#36253=CARTESIAN_POINT('Ctrl Pts',(-7.40772485187387E-16,0.509367536895501,
-0.920811872709318));
#36254=CARTESIAN_POINT('Ctrl Pts',(-2.46291782561222E-15,0.516359973174507,
-0.91563084291723));
#36255=CARTESIAN_POINT('Ctrl Pts',(-2.42861286636753E-15,0.523284879313264,
-0.910365918516622));
#36256=CARTESIAN_POINT('Ctrl Pts',(-2.25061356671081E-15,0.559216373476985,
-0.883047627613864));
#36257=CARTESIAN_POINT('Ctrl Pts',(-2.96823005161294E-16,0.593340067182582,
-0.853468264465714));
#36258=CARTESIAN_POINT('Ctrl Pts',(-6.03683769639929E-16,0.625471482738123,
-0.821855359183385));
#36259=CARTESIAN_POINT('Ctrl Pts',(-9.08089369103446E-16,0.657345817765653,
-0.790495385875619));
#36260=CARTESIAN_POINT('Ctrl Pts',(2.15765114517466E-16,0.687260208276574,
-0.757133177797282));
#36261=CARTESIAN_POINT('Ctrl Pts',(5.89805981832114E-16,0.714989723653526,
-0.721967245339149));
#36262=CARTESIAN_POINT('Ctrl Pts',(7.57871803351495E-16,0.727449281390145,
-0.70616632131044));
#36263=CARTESIAN_POINT('Ctrl Pts',(1.44173626698327E-16,0.739467070861113,
-0.690001019680507));
#36264=CARTESIAN_POINT('Ctrl Pts',(1.59594559789866E-16,0.751019236986007,
-0.673488664556055));
#36265=CARTESIAN_POINT('Ctrl Pts',(1.69123973183035E-16,0.758157933842884,
-0.663284803535346));
#36266=CARTESIAN_POINT('Ctrl Pts',(-8.8777281847663E-16,0.765118780990856,
-0.652948409395475));
#36267=CARTESIAN_POINT('Ctrl Pts',(-9.47159017883337E-16,0.771895701092293,
-0.642483556554596));
#36268=CARTESIAN_POINT('Ctrl Pts',(-9.8353236423952E-16,0.77604648468411,
-0.636073957678923));
#36269=CARTESIAN_POINT('Ctrl Pts',(-6.35014032128769E-16,0.780127059785162,
-0.629617905044286));
#36270=CARTESIAN_POINT('Ctrl Pts',(-6.90419943438769E-16,0.784131582650059,
-0.623124085326683));
#36271=CARTESIAN_POINT('Ctrl Pts',(-1.0034507112653E-15,0.806756223911961,
-0.586435484340496));
#36272=CARTESIAN_POINT('Ctrl Pts',(-2.58467719790652E-15,0.827002143027744,
-0.548473780018055));
#36273=CARTESIAN_POINT('Ctrl Pts',(-2.08860706507608E-15,0.8446799545592,
-0.50942695250173));
#36274=CARTESIAN_POINT('Ctrl Pts',(-1.61028094156565E-15,0.861725445715345,
-0.471776796999125));
#36275=CARTESIAN_POINT('Ctrl Pts',(-2.43875266999451E-15,0.876383418703462,
-0.433116863243482));
#36276=CARTESIAN_POINT('Ctrl Pts',(-2.39912256727592E-15,0.888437242092163,
-0.393609940259947));
#36277=CARTESIAN_POINT('Ctrl Pts',(-2.36446274816928E-15,0.898979312627847,
-0.359057852071011));
#36278=CARTESIAN_POINT('Ctrl Pts',(-1.01325357859657E-15,0.907528950391913,
-0.323857499715885));
#36279=CARTESIAN_POINT('Ctrl Pts',(-1.02695629777827E-15,0.913908649078052,
-0.288121577880467));
#36280=CARTESIAN_POINT('Ctrl Pts',(-0.0548926501499415,-1.2158567361346,
0.000987498914498598));
#36281=CARTESIAN_POINT('Ctrl Pts',(-0.0365951000999603,-1.21332229077892,
-0.308813117966906));
#36282=CARTESIAN_POINT('Ctrl Pts',(-0.0182975500499791,-1.08971454031158,
-0.620549786380947));
#36283=CARTESIAN_POINT('Ctrl Pts',(2.23779328401008E-15,-0.876385019502642,
-0.844404278593208));
#36284=CARTESIAN_POINT('',(-7.785,-0.556433207999828,-0.780144311992993));
#36285=CARTESIAN_POINT('Ctrl Pts',(-7.785,-0.5576340527839,-0.781217367305846));
#36286=CARTESIAN_POINT('Ctrl Pts',(-7.785,-0.578747991216662,-0.770087997067624));
#36287=CARTESIAN_POINT('Ctrl Pts',(-7.785,-0.5993761820992,-0.758139560309488));
#36288=CARTESIAN_POINT('Ctrl Pts',(-7.785,-0.619465300627149,-0.745383173566744));
#36289=CARTESIAN_POINT('Ctrl Pts',(-7.785,-0.655692140857232,-0.722379497034115));
#36290=CARTESIAN_POINT('Ctrl Pts',(-7.785,-0.690167491685533,-0.696752077864181));
#36291=CARTESIAN_POINT('Ctrl Pts',(-7.785,-0.722812205716661,-0.668816216966533));
#36292=CARTESIAN_POINT('Ctrl Pts',(-7.785,-0.7335642421842,-0.659615113387031));
#36293=CARTESIAN_POINT('Ctrl Pts',(-7.785,-0.744117533296352,-0.650163120371217));
#36294=CARTESIAN_POINT('Ctrl Pts',(-7.785,-0.754468725562236,-0.640470210083598));
#36295=CARTESIAN_POINT('Ctrl Pts',(-7.785,-0.763826437854487,-0.631707599611654));
#36296=CARTESIAN_POINT('Ctrl Pts',(-7.785,-0.773020919233301,-0.622745822047555));
#36297=CARTESIAN_POINT('Ctrl Pts',(-7.785,-0.782032296561331,-0.613610157430372));
#36298=CARTESIAN_POINT('Ctrl Pts',(-7.785,-0.812493295643311,-0.582729032227493));
#36299=CARTESIAN_POINT('Ctrl Pts',(-7.785,-0.840906423243611,-0.549826817131425));
#36300=CARTESIAN_POINT('Ctrl Pts',(-7.785,-0.867192555862543,-0.515209435590686));
#36301=CARTESIAN_POINT('Ctrl Pts',(-7.785,-0.884711533165385,-0.492137912278838));
#36302=CARTESIAN_POINT('Ctrl Pts',(-7.785,-0.901285379133529,-0.468303396752018));
#36303=CARTESIAN_POINT('Ctrl Pts',(-7.785,-0.916884395328298,-0.443785427125382));
#36304=CARTESIAN_POINT('Ctrl Pts',(-7.785,-0.922043717372295,-0.435676191287086));
#36305=CARTESIAN_POINT('Ctrl Pts',(-7.785,-0.927096351428236,-0.427492128011766));
#36306=CARTESIAN_POINT('Ctrl Pts',(-7.785,-0.932041071713118,-0.419235942078489));
#36307=CARTESIAN_POINT('Ctrl Pts',(-7.785,-0.93698833006316,-0.410975518344757));
#36308=CARTESIAN_POINT('Ctrl Pts',(-7.785,-0.941823150759485,-0.402650204861208));
#36309=CARTESIAN_POINT('Ctrl Pts',(-7.785,-0.946543129270692,-0.394266174047561));
#36310=CARTESIAN_POINT('Ctrl Pts',(-7.785,-0.969144618968524,-0.354119468800706));
#36311=CARTESIAN_POINT('Ctrl Pts',(-7.785,-0.989128076220463,-0.312608831398347));
#36312=CARTESIAN_POINT('Ctrl Pts',(-7.785,-1.0064033332032,-0.270063237970165));
#36313=CARTESIAN_POINT('Ctrl Pts',(-7.785,-1.02365060027322,-0.227586578245705));
#36314=CARTESIAN_POINT('Ctrl Pts',(-7.785,-1.03819918540846,-0.184077227350852));
#36315=CARTESIAN_POINT('Ctrl Pts',(-7.785,-1.04992333380568,-0.139823354894582));
#36316=CARTESIAN_POINT('Ctrl Pts',(-7.785,-1.05579967799946,-0.11764255526207));
#36317=CARTESIAN_POINT('Ctrl Pts',(-7.785,-1.06096583628138,-0.0952742038286101));
#36318=CARTESIAN_POINT('Ctrl Pts',(-7.785,-1.0654016453404,-0.0727521974605108));
#36319=CARTESIAN_POINT('Ctrl Pts',(-7.785,-1.06730690665633,-0.0630785828122528));
#36320=CARTESIAN_POINT('Ctrl Pts',(-7.785,-1.06907738892517,-0.0533766060944693));
#36321=CARTESIAN_POINT('Ctrl Pts',(-7.785,-1.07071130661907,-0.0436488970915968));
#36322=CARTESIAN_POINT('Ctrl Pts',(-7.785,-1.07200966230447,-0.0359189934759291));
#36323=CARTESIAN_POINT('Ctrl Pts',(-7.785,-1.07322141063688,-0.0281746421691217));
#36324=CARTESIAN_POINT('Ctrl Pts',(-7.785,-1.07434459151835,-0.0204264539147781));
#36325=CARTESIAN_POINT('Ctrl Pts',(-7.785,-1.0811257447752,0.0263528786774973));
#36326=CARTESIAN_POINT('Ctrl Pts',(-7.785,-1.08469796082786,0.0733627252990918));
#36327=CARTESIAN_POINT('Ctrl Pts',(-7.785,-1.08495012712384,0.120289602356072));
#36328=CARTESIAN_POINT('Ctrl Pts',(-7.785,-1.08497075310017,0.124127992620137));
#36329=CARTESIAN_POINT('Ctrl Pts',(-7.785,-1.08496914232922,0.127965843592304));
#36330=CARTESIAN_POINT('Ctrl Pts',(-7.785,-1.08494522067707,0.131802991509847));
#36331=CARTESIAN_POINT('Ctrl Pts',(-7.785,-1.08466326798781,0.177029557276298));
#36332=CARTESIAN_POINT('Ctrl Pts',(-7.785,-1.08128615140463,0.222157593215046));
#36333=CARTESIAN_POINT('Ctrl Pts',(-7.785,-1.07500410468562,0.266979872471771));
#36334=CARTESIAN_POINT('Ctrl Pts',(-7.785,-1.07185759882872,0.289430129610702));
#36335=CARTESIAN_POINT('Ctrl Pts',(-7.785,-1.06798150946743,0.311803845021642));
#36336=CARTESIAN_POINT('Ctrl Pts',(-7.785,-1.06339502635409,0.334075419501835));
#36337=CARTESIAN_POINT('Ctrl Pts',(-7.785,-1.06102777465901,0.345570593720789));
#36338=CARTESIAN_POINT('Ctrl Pts',(-7.785,-1.05847122649056,0.357038558179951));
#36339=CARTESIAN_POINT('Ctrl Pts',(-7.785,-1.05572770902942,0.368475774034161));
#36340=CARTESIAN_POINT('Ctrl Pts',(-7.785,-1.05326681078295,0.378734802758733));
#36341=CARTESIAN_POINT('Ctrl Pts',(-7.785,-1.0506549099214,0.388970584699868));
#36342=CARTESIAN_POINT('Ctrl Pts',(-7.785,-1.04789957705921,0.399160050513257));
#36343=CARTESIAN_POINT('Ctrl Pts',(-7.785,-1.0355261113626,0.44491822639059));
#36344=CARTESIAN_POINT('Ctrl Pts',(-7.785,-1.0202432411082,0.489835263872287));
#36345=CARTESIAN_POINT('Ctrl Pts',(-7.785,-1.00227600753725,0.533685063338825));
#36346=CARTESIAN_POINT('Ctrl Pts',(-7.785,-0.983902194037811,0.578527138453172));
#36347=CARTESIAN_POINT('Ctrl Pts',(-7.785,-0.962720954482079,0.622254138907397));
#36348=CARTESIAN_POINT('Ctrl Pts',(-7.785,-0.938918185991045,0.664625763107378));
#36349=CARTESIAN_POINT('Ctrl Pts',(-7.785,-0.926738910664416,0.686306252810178));
#36350=CARTESIAN_POINT('Ctrl Pts',(-7.785,-0.913872435977145,0.707631818960279));
#36351=CARTESIAN_POINT('Ctrl Pts',(-7.785,-0.900338597033089,0.728569055025174));
#36352=CARTESIAN_POINT('Ctrl Pts',(-7.785,-0.89089399903829,0.743180118343761));
#36353=CARTESIAN_POINT('Ctrl Pts',(-7.785,-0.88112432730713,0.75760204684153));
#36354=CARTESIAN_POINT('Ctrl Pts',(-7.785,-0.871035410752641,0.771823051085395));
#36355=CARTESIAN_POINT('Ctrl Pts',(-7.785,-0.865701397585292,0.77934170023667));
#36356=CARTESIAN_POINT('Ctrl Pts',(-7.785,-0.86027823994916,0.786803846419087));
#36357=CARTESIAN_POINT('Ctrl Pts',(-7.785,-0.854775425221195,0.794196577713452));
#36358=CARTESIAN_POINT('Ctrl Pts',(-7.785,-0.824631208231136,0.834693688247454));
#36359=CARTESIAN_POINT('Ctrl Pts',(-7.785,-0.792039562878693,0.873196157076302));
#36360=CARTESIAN_POINT('Ctrl Pts',(-7.785,-0.757211887306745,0.909454779884878));
#36361=CARTESIAN_POINT('Ctrl Pts',(-7.785,-0.722636821016273,0.945450414581139));
#36362=CARTESIAN_POINT('Ctrl Pts',(-7.785,-0.685857497318535,0.979235714907832));
#36363=CARTESIAN_POINT('Ctrl Pts',(-7.785,-0.647033561635485,1.01054947663034));
#36364=CARTESIAN_POINT('Ctrl Pts',(-7.785,-0.610160681532922,1.04028959857419));
#36365=CARTESIAN_POINT('Ctrl Pts',(-7.785,-0.571442820559113,1.06780104655221));
#36366=CARTESIAN_POINT('Ctrl Pts',(-7.785,-0.530983509300133,1.09283187766981));
#36367=CARTESIAN_POINT('Ctrl Pts',(-7.785,-0.557634052783907,-0.781217367305842));
#36368=CARTESIAN_POINT('Ctrl Pts',(-7.7629409778209,-0.31739492458004,-0.950718299157138));
#36369=CARTESIAN_POINT('Ctrl Pts',(-7.71705842806939,0.358267300689441,
-1.06099670633061));
#36370=CARTESIAN_POINT('Ctrl Pts',(-7.64735235074545,1.09209582283259,-0.300632258159738));
#36371=CARTESIAN_POINT('Ctrl Pts',(-7.5758817680282,0.844510306117659,0.755061250975084));
#36372=CARTESIAN_POINT('Ctrl Pts',(-7.50441118531095,-0.17668969425852,
1.11881329398577));
#36373=CARTESIAN_POINT('Ctrl Pts',(-7.44682637322301,-0.869040033824089,
0.586431559724317));
#36374=CARTESIAN_POINT('Ctrl Pts',(-7.41306508870749,-0.957373000383943,
0.133844055008089));
#36375=CARTESIAN_POINT('Ctrl Pts',(-7.40312733176438,-0.956848572177365,
0.000426154272836167));
#36376=CARTESIAN_POINT('Origin',(-7.785,-1.13809670924099E-16,0.));
#36377=CARTESIAN_POINT('',(-7.785,-1.215,-1.48794586096403E-16));
#36378=CARTESIAN_POINT('Origin',(-7.785,0.,0.));
#36379=CARTESIAN_POINT('Origin',(-7.785,0.,0.));
#36380=CARTESIAN_POINT('',(-7.785,0.556433207999845,-0.780144311992981));
#36381=CARTESIAN_POINT('Ctrl Pts',(-7.785,0.532258410758877,1.09442686519077));
#36382=CARTESIAN_POINT('Ctrl Pts',(-7.785,0.557739637633036,1.07882088466419));
#36383=CARTESIAN_POINT('Ctrl Pts',(-7.785,0.582563623672786,1.06223431603398));
#36384=CARTESIAN_POINT('Ctrl Pts',(-7.785,0.60666536531996,1.04466370008905));
#36385=CARTESIAN_POINT('Ctrl Pts',(-7.785,0.645212441942324,1.01656216746761));
#36386=CARTESIAN_POINT('Ctrl Pts',(-7.785,0.681913950695198,0.985944425966533));
#36387=CARTESIAN_POINT('Ctrl Pts',(-7.785,0.716645235920004,0.953067759411124));
#36388=CARTESIAN_POINT('Ctrl Pts',(-7.785,0.735328952881038,0.935381735742042));
#36389=CARTESIAN_POINT('Ctrl Pts',(-7.785,0.753441909891504,0.917041571835294));
#36390=CARTESIAN_POINT('Ctrl Pts',(-7.785,0.770960226206176,0.898085195601122));
#36391=CARTESIAN_POINT('Ctrl Pts',(-7.785,0.778530501447049,0.889893484532288));
#36392=CARTESIAN_POINT('Ctrl Pts',(-7.785,0.785989449819457,0.881586755557057));
#36393=CARTESIAN_POINT('Ctrl Pts',(-7.785,0.793326100456532,0.873178793404179));
#36394=CARTESIAN_POINT('Ctrl Pts',(-7.785,0.826126511808265,0.835588804336062));
#36395=CARTESIAN_POINT('Ctrl Pts',(-7.785,0.856535186295519,0.795925149890432));
#36396=CARTESIAN_POINT('Ctrl Pts',(-7.785,0.884405829267192,0.754483325808291));
#36397=CARTESIAN_POINT('Ctrl Pts',(-7.785,0.901804029846728,0.728613338937312));
#36398=CARTESIAN_POINT('Ctrl Pts',(-7.785,0.918212284704953,0.702049892369393));
#36399=CARTESIAN_POINT('Ctrl Pts',(-7.785,0.933585061142037,0.674862130976118));
#36400=CARTESIAN_POINT('Ctrl Pts',(-7.785,0.94077358376822,0.66214875816863));
#36401=CARTESIAN_POINT('Ctrl Pts',(-7.785,0.947735571875419,0.649298856397));
#36402=CARTESIAN_POINT('Ctrl Pts',(-7.785,0.95446575102645,0.63631947094407));
#36403=CARTESIAN_POINT('Ctrl Pts',(-7.785,0.958975356722034,0.627622538923361));
#36404=CARTESIAN_POINT('Ctrl Pts',(-7.785,0.96337845490693,0.61887200525621));
#36405=CARTESIAN_POINT('Ctrl Pts',(-7.785,0.967670436201489,0.610077271220812));
#36406=CARTESIAN_POINT('Ctrl Pts',(-7.785,0.988967668483222,0.566436938061539));
#36407=CARTESIAN_POINT('Ctrl Pts',(-7.785,1.00756077659699,0.521655942866011));
#36408=CARTESIAN_POINT('Ctrl Pts',(-7.785,1.02330935649198,0.476005300563686));
#36409=CARTESIAN_POINT('Ctrl Pts',(-7.785,1.0386172582705,0.431632058458665));
#36410=CARTESIAN_POINT('Ctrl Pts',(-7.785,1.05123767834139,0.386436094961105));
#36411=CARTESIAN_POINT('Ctrl Pts',(-7.785,1.06099323746147,0.340664258919277));
#36412=CARTESIAN_POINT('Ctrl Pts',(-7.785,1.06608164654541,0.316790094103385));
#36413=CARTESIAN_POINT('Ctrl Pts',(-7.785,1.07038983391497,0.292759321382559));
#36414=CARTESIAN_POINT('Ctrl Pts',(-7.785,1.07388705755652,0.268608144583126));
#36415=CARTESIAN_POINT('Ctrl Pts',(-7.785,1.07594738847747,0.254379881984722));
#36416=CARTESIAN_POINT('Ctrl Pts',(-7.785,1.07772617782379,0.240109850761259));
#36417=CARTESIAN_POINT('Ctrl Pts',(-7.785,1.07921648757224,0.225805690334931));
#36418=CARTESIAN_POINT('Ctrl Pts',(-7.785,1.08013730941692,0.216967538800246));
#36419=CARTESIAN_POINT('Ctrl Pts',(-7.785,1.08094784771634,0.208116602027595));
#36420=CARTESIAN_POINT('Ctrl Pts',(-7.785,1.08164565231098,0.199268521621097));
#36421=CARTESIAN_POINT('Ctrl Pts',(-7.785,1.08521244038656,0.154042067212324));
#36422=CARTESIAN_POINT('Ctrl Pts',(-7.785,1.08584829648986,0.108797261783825));
#36423=CARTESIAN_POINT('Ctrl Pts',(-7.785,1.08340106664489,0.0637641771385276));
#36424=CARTESIAN_POINT('Ctrl Pts',(-7.785,1.08315610349527,0.0592564492377615));
#36425=CARTESIAN_POINT('Ctrl Pts',(-7.785,1.08288020632508,0.0547508504375447));
#36426=CARTESIAN_POINT('Ctrl Pts',(-7.785,1.08257319383316,0.0502476177093405));
#36427=CARTESIAN_POINT('Ctrl Pts',(-7.785,1.07966075959026,0.00752828365533442));
#36428=CARTESIAN_POINT('Ctrl Pts',(-7.785,1.07395105666554,-0.0349795970626121));
#36429=CARTESIAN_POINT('Ctrl Pts',(-7.785,1.06556613520383,-0.0770620868862156));
#36430=CARTESIAN_POINT('Ctrl Pts',(-7.785,1.06139056925744,-0.0980185397580686));
#36431=CARTESIAN_POINT('Ctrl Pts',(-7.785,1.05655104212579,-0.118869222739669));
#36432=CARTESIAN_POINT('Ctrl Pts',(-7.785,1.05105978648461,-0.139585623514728));
#36433=CARTESIAN_POINT('Ctrl Pts',(-7.785,1.04643720856273,-0.157024836529205));
#36434=CARTESIAN_POINT('Ctrl Pts',(-7.785,1.04135275390333,-0.174368872848005));
#36435=CARTESIAN_POINT('Ctrl Pts',(-7.785,1.03581286032973,-0.191599736380545));
#36436=CARTESIAN_POINT('Ctrl Pts',(-7.785,1.03314821815863,-0.199887636681043));
#36437=CARTESIAN_POINT('Ctrl Pts',(-7.785,1.0303812524574,-0.208139819618536));
#36438=CARTESIAN_POINT('Ctrl Pts',(-7.785,1.02751360825937,-0.216353690840345));
#36439=CARTESIAN_POINT('Ctrl Pts',(-7.785,1.01263586389863,-0.258968418404492));
#36440=CARTESIAN_POINT('Ctrl Pts',(-7.785,0.995049070732015,-0.300562539231134));
#36441=CARTESIAN_POINT('Ctrl Pts',(-7.785,0.97491261572845,-0.340890293089778));
#36442=CARTESIAN_POINT('Ctrl Pts',(-7.785,0.954937271641593,-0.380895386311694));
#36443=CARTESIAN_POINT('Ctrl Pts',(-7.785,0.9324520326871,-0.419655189247156));
#36444=CARTESIAN_POINT('Ctrl Pts',(-7.785,0.907576185682416,-0.456894436402826));
#36445=CARTESIAN_POINT('Ctrl Pts',(-7.785,0.896398825208152,-0.473626991847904));
#36446=CARTESIAN_POINT('Ctrl Pts',(-7.785,0.884738404704367,-0.490051998613649));
#36447=CARTESIAN_POINT('Ctrl Pts',(-7.785,0.872604028769965,-0.506141415467363));
#36448=CARTESIAN_POINT('Ctrl Pts',(-7.785,0.865105828753884,-0.516083555579341));
#36449=CARTESIAN_POINT('Ctrl Pts',(-7.785,0.857426636030853,-0.525897514492815));
#36450=CARTESIAN_POINT('Ctrl Pts',(-7.785,0.84956844738637,-0.535576253967916));
#36451=CARTESIAN_POINT('Ctrl Pts',(-7.785,0.844755476884386,-0.541504272458888));
#36452=CARTESIAN_POINT('Ctrl Pts',(-7.785,0.839876635612896,-0.547379881046622));
#36453=CARTESIAN_POINT('Ctrl Pts',(-7.785,0.834938380506431,-0.553194836113957));
#36454=CARTESIAN_POINT('Ctrl Pts',(-7.785,0.807036952950441,-0.586049669259403));
#36455=CARTESIAN_POINT('Ctrl Pts',(-7.785,0.777189661728921,-0.617035617704938));
#36456=CARTESIAN_POINT('Ctrl Pts',(-7.785,0.745516763485908,-0.645914476150201));
#36457=CARTESIAN_POINT('Ctrl Pts',(-7.785,0.714976782555787,-0.673760358122703));
#36458=CARTESIAN_POINT('Ctrl Pts',(-7.785,0.682738657926675,-0.699647618275338));
#36459=CARTESIAN_POINT('Ctrl Pts',(-7.785,0.648890268218106,-0.723319923617524));
#36460=CARTESIAN_POINT('Ctrl Pts',(-7.785,0.619286115682046,-0.744023967274078));
#36461=CARTESIAN_POINT('Ctrl Pts',(-7.785,0.588449651909176,-0.763033317509813));
#36462=CARTESIAN_POINT('Ctrl Pts',(-7.785,0.556433207999864,-0.780144311992967));
#36463=CARTESIAN_POINT('Origin',(-7.785,0.,0.));
#36464=CARTESIAN_POINT('Origin',(-8.61687266823562,0.,0.));
#36465=CARTESIAN_POINT('Ctrl Pts',(-7.785,0.556433207999845,-0.780144311992981));
#36466=CARTESIAN_POINT('Ctrl Pts',(-7.76117647242759,0.815939785066093,
-0.595052816798781));
#36467=CARTESIAN_POINT('Ctrl Pts',(-7.71352941728275,1.13124973052358,0.0512203649262202));
#36468=CARTESIAN_POINT('Ctrl Pts',(-7.64205883456552,0.569045812913815,
0.980302233127841));
#36469=CARTESIAN_POINT('Ctrl Pts',(-7.57058825184826,-0.514804186274824,
1.00861045471588));
#36470=CARTESIAN_POINT('Ctrl Pts',(-7.52052619640497,-0.943555255514336,
0.382401100605641));
#36471=CARTESIAN_POINT('Ctrl Pts',(-7.49428766853409,-0.959633789666665,
0.0328156789457131));
#36472=CARTESIAN_POINT('Ctrl Pts',(-7.49187266823563,-0.959412934693052,
0.000617836956614886));
#36473=CARTESIAN_POINT('Ctrl Pts',(-7.93323468161444,0.705521886480338,
-0.989173325407244));
#36474=CARTESIAN_POINT('Ctrl Pts',(-7.90941115404203,1.03455970660609,-0.754489092001615));
#36475=CARTESIAN_POINT('Ctrl Pts',(-7.8617640988972,1.43435264553733,0.0649441621553011));
#36476=CARTESIAN_POINT('Ctrl Pts',(-7.79029351617995,0.721513866621781,
1.24296082781143));
#36477=CARTESIAN_POINT('Ctrl Pts',(-7.7188229334627,-0.652738936941171,
1.27885385074857));
#36478=CARTESIAN_POINT('Ctrl Pts',(-7.64735235074546,-1.42884542185819,
0.145316990997596));
#36479=CARTESIAN_POINT('Ctrl Pts',(-7.5758817680282,-0.896443945405535,
-1.12228602947411));
#36480=CARTESIAN_POINT('Ctrl Pts',(-7.50441118531097,0.457089628791888,
-1.36148449659785));
#36481=CARTESIAN_POINT('Ctrl Pts',(-7.4329406025937,1.3919330456215,-0.353977390791757));
#36482=CARTESIAN_POINT('Ctrl Pts',(-7.36147001987648,1.05193816003137,0.977876750342409));
#36483=CARTESIAN_POINT('Ctrl Pts',(-7.28999943715921,-0.25153214713002,
1.41402569308405));
#36484=CARTESIAN_POINT('Ctrl Pts',(-7.21852885444197,-1.32461931868978,
0.555117463789919));
#36485=CARTESIAN_POINT('Ctrl Pts',(-7.14705827172472,-1.18450017731315,
-0.81223974728715));
#36486=CARTESIAN_POINT('Ctrl Pts',(-7.07558768900747,0.0404963929544019,
-1.43566122947319));
#36487=CARTESIAN_POINT('Ctrl Pts',(-7.00411710629023,1.22840163452736,-0.744176158150377));
#36488=CARTESIAN_POINT('Ctrl Pts',(-6.93264652357298,1.29122272974647,0.628897789905487));
#36489=CARTESIAN_POINT('Ctrl Pts',(-6.86117594085574,0.171421495630961,
1.42596696158188));
#36490=CARTESIAN_POINT('Ctrl Pts',(-6.78970535813848,-1.10538337312329,
0.917003589837982));
#36491=CARTESIAN_POINT('Ctrl Pts',(-6.71823477542124,-1.36977524784193,
-0.431837537599902));
#36492=CARTESIAN_POINT('Ctrl Pts',(-6.64676419270399,-0.379599306735098,
-1.38516138616941));
#36493=CARTESIAN_POINT('Ctrl Pts',(-6.57529360998674,0.958249021520171,
-1.06982552176842));
#36494=CARTESIAN_POINT('Ctrl Pts',(-6.5038230272695,1.41844363852531,0.225356282468531));
#36495=CARTESIAN_POINT('Ctrl Pts',(-6.43235244455225,0.579495426924149,
1.31413577551544));
#36496=CARTESIAN_POINT('Ctrl Pts',(-6.360881861835,-0.790208678038612,1.19930732160193));
#36497=CARTESIAN_POINT('Ctrl Pts',(-6.28941127911776,-1.43616606331737,
-0.0139585114361597));
#36498=CARTESIAN_POINT('Ctrl Pts',(-6.2179406964005,-0.766748777246146,
-1.21443983438033));
#36499=CARTESIAN_POINT('Ctrl Pts',(-6.14647011368326,0.60492846703713,-1.30262402536569));
#36500=CARTESIAN_POINT('Ctrl Pts',(-6.07499953096601,1.42255586777629,-0.197743783258168));
#36501=CARTESIAN_POINT('Ctrl Pts',(-6.00352894824877,0.937274082844972,
1.08824863615832));
#36502=CARTESIAN_POINT('Ctrl Pts',(-5.93205836553151,-0.406450621262066,
1.37752157637255));
#36503=CARTESIAN_POINT('Ctrl Pts',(-5.86058778281429,-1.37790998250129,
0.405131930188321));
#36504=CARTESIAN_POINT('Ctrl Pts',(-5.789117200097,-1.08735101901064,-0.93831527865966));
#36505=CARTESIAN_POINT('Ctrl Pts',(-5.71764661737979,0.199105302652743,
-1.42236594420155));
#36506=CARTESIAN_POINT('Ctrl Pts',(-5.64617603466251,1.3032024399867,-0.603681373867629));
#36507=CARTESIAN_POINT('Ctrl Pts',(-5.57470545194529,1.21370537961352,0.767910836124945));
#36508=CARTESIAN_POINT('Ctrl Pts',(-5.50323486922803,0.0125838667550361,
1.43617876569961));
#36509=CARTESIAN_POINT('Ctrl Pts',(-5.43176428651079,-1.2000631235608,0.789060390726951));
#36510=CARTESIAN_POINT('Ctrl Pts',(-5.36029370379354,-1.31358051036201,
-0.580752997015039));
#36511=CARTESIAN_POINT('Ctrl Pts',(-5.28882312107629,-0.223998495813416,
-1.41865868855736));
#36512=CARTESIAN_POINT('Ctrl Pts',(-5.21735253835905,1.07074220835543,-0.957224594330622));
#36513=CARTESIAN_POINT('Ctrl Pts',(-5.1458819556418,1.3847974503765,0.380924956095192));
#36514=CARTESIAN_POINT('Ctrl Pts',(-5.07441137292455,0.430526182985665,
1.37018794568822));
#36515=CARTESIAN_POINT('Ctrl Pts',(-5.00294079020731,-0.918061069553906,
1.10450517124862));
#36516=CARTESIAN_POINT('Ctrl Pts',(-4.93147020749005,-1.42580247026315,
-0.172786332031617));
#36517=CARTESIAN_POINT('Ctrl Pts',(-4.85999962477281,-0.627661144420497,
-1.29182401608353));
#36518=CARTESIAN_POINT('Ctrl Pts',(-4.78852904205556,0.745350728865686,
-1.22768892302766));
#36519=CARTESIAN_POINT('Ctrl Pts',(-4.71705845933832,1.43570096959843,-0.0391219457536234));
#36520=CARTESIAN_POINT('Ctrl Pts',(-4.64558787662107,0.811102515967952,
1.18527655394675));
#36521=CARTESIAN_POINT('Ctrl Pts',(-4.57411729390382,-0.556379182120533,
1.32408836806624));
#36522=CARTESIAN_POINT('Ctrl Pts',(-4.50264671118658,-1.41427699429376,
0.250176705863753));
#36523=CARTESIAN_POINT('Ctrl Pts',(-4.43117612846932,-0.976848184493127,
-1.05287008942125));
#36524=CARTESIAN_POINT('Ctrl Pts',(-4.35970554575208,0.355269193463592,
-1.39160037400151));
#36525=CARTESIAN_POINT('Ctrl Pts',(-4.28823496303483,1.36199794803372,-0.455773397970269));
#36526=CARTESIAN_POINT('Ctrl Pts',(-4.21676438031759,1.12128210138353,0.897493314661654));
#36527=CARTESIAN_POINT('Ctrl Pts',(-4.14529379760033,-0.146408349622836,
1.42875204143551));
#36528=CARTESIAN_POINT('Ctrl Pts',(-4.07382321488309,-1.28000439499941,
0.651426549602967));
#36529=CARTESIAN_POINT('Ctrl Pts',(-4.00235263216585,-1.24125317334416,
-0.722536061666472));
#36530=CARTESIAN_POINT('Ctrl Pts',(-3.93088204944859,-0.06564666341837,
-1.43473283796234));
#36531=CARTESIAN_POINT('Ctrl Pts',(-3.85941146673135,1.17008517634921,-0.832867625036097));
#36532=CARTESIAN_POINT('Ctrl Pts',(-3.78794088401411,1.33414400933146,0.531815346817302));
#36533=CARTESIAN_POINT('Ctrl Pts',(-3.71647030129685,0.276269472961998,
1.40941228143319));
#36534=CARTESIAN_POINT('Ctrl Pts',(-3.64499971857961,-1.03463838333717,
0.996138151297738));
#36535=CARTESIAN_POINT('Ctrl Pts',(-3.57352913586236,-1.39792802378473,
-0.329492095599789));
#36536=CARTESIAN_POINT('Ctrl Pts',(-3.50205855314511,-0.480864952480873,
-1.35334278666603));
#36537=CARTESIAN_POINT('Ctrl Pts',(-3.43058797042787,0.876619038512565,
-1.13767607958625));
#36538=CARTESIAN_POINT('Ctrl Pts',(-3.35911738771062,1.431213650342,0.119980364310839));
#36539=CARTESIAN_POINT('Ctrl Pts',(-3.28764680499337,0.674969472810977,
1.2677476134936));
#36540=CARTESIAN_POINT('Ctrl Pts',(-3.21617622227613,-0.699474626432212,
1.25439349795945));
#36541=CARTESIAN_POINT('Ctrl Pts',(-3.14470563955887,-1.43327470143649,
0.0921489607514472));
#36542=CARTESIAN_POINT('Ctrl Pts',(-3.07323505684163,-0.854348284485474,
-1.15449417908544));
#36543=CARTESIAN_POINT('Ctrl Pts',(-3.00176447412438,0.507069880402349,
-1.34374399985048));
#36544=CARTESIAN_POINT('Ctrl Pts',(-2.93029389140714,1.40406621142284,-0.302267885634783));
#36545=CARTESIAN_POINT('Ctrl Pts',(-2.85882330868989,1.01508790663436,1.01605331678519));
#36546=CARTESIAN_POINT('Ctrl Pts',(-2.78735272597264,-0.303602466166582,
1.40377823864132));
#36547=CARTESIAN_POINT('Ctrl Pts',(-2.71588214325539,-1.34422541758585,
0.505792276988717));
#36548=CARTESIAN_POINT('Ctrl Pts',(-2.64441156053815,-1.15368150681488,
-0.855445370306784));
#36549=CARTESIAN_POINT('Ctrl Pts',(-2.5729409778209,0.0935114020565075,
-1.4331864562681));
#36550=CARTESIAN_POINT('Ctrl Pts',(-2.50147039510365,1.25505785762914,-0.698281873420766));
#36551=CARTESIAN_POINT('Ctrl Pts',(-2.4299998123864,1.26710540905413,0.676174299345015));
#36552=CARTESIAN_POINT('Ctrl Pts',(-2.35852922966916,0.118619786410601,
1.43132705801742));
#36553=CARTESIAN_POINT('Ctrl Pts',(-2.28705864695191,-1.13850888695148,
0.875537158020446));
#36554=CARTESIAN_POINT('Ctrl Pts',(-2.21558806423466,-1.35288506094146,
-0.482151234210018));
#36555=CARTESIAN_POINT('Ctrl Pts',(-2.14411748151742,-0.328163064620681,
-1.39824061009842));
#36556=CARTESIAN_POINT('Ctrl Pts',(-2.07264689880017,0.997121237106055,
-1.03369097860381));
#36557=CARTESIAN_POINT('Ctrl Pts',(-2.00117631608292,1.40914902059169,0.277609147294719));
#36558=CARTESIAN_POINT('Ctrl Pts',(-1.92970573336567,0.530546857965926,
1.33464895458537));
#36559=CARTESIAN_POINT('Ctrl Pts',(-1.85823515064843,-0.833979541327682,
1.16929291685568));
#36560=CARTESIAN_POINT('Ctrl Pts',(-1.78676456793118,-1.43466978575981,
-0.0670105030551046));
#36561=CARTESIAN_POINT('Ctrl Pts',(-1.71529398521393,-0.72135578893274,
-1.24193946088825));
#36562=CARTESIAN_POINT('Ctrl Pts',(-1.64382340249668,0.652643037024826,
-1.27938456598828));
#36563=CARTESIAN_POINT('Ctrl Pts',(-1.57235281977944,1.42889057506806,-0.145050098163382));
#36564=CARTESIAN_POINT('Ctrl Pts',(-1.50088223706219,0.896427004851561,
1.12213475629642));
#36565=CARTESIAN_POINT('Ctrl Pts',(-1.42941165434495,-0.457067910847659,
1.36156407656574));
#36566=CARTESIAN_POINT('Ctrl Pts',(-1.3579410716277,-1.39193748201553,0.353946154706768));
#36567=CARTESIAN_POINT('Ctrl Pts',(-1.28647048891045,-1.05194098533954,
-0.977848588878373));
#36568=CARTESIAN_POINT('Ctrl Pts',(-1.2149999061932,0.25152096267351,-1.414038575788));
#36569=CARTESIAN_POINT('Ctrl Pts',(-1.14352932347596,1.32461677048183,-0.555120164209031));
#36570=CARTESIAN_POINT('Ctrl Pts',(-1.07205874075871,1.18450478400261,0.812228737094626));
#36571=CARTESIAN_POINT('Ctrl Pts',(-1.00058815804146,-0.0404863500284713,
1.43566340881953));
#36572=CARTESIAN_POINT('Ctrl Pts',(-0.929117575324211,-1.22839760243372,
0.744182813832753));
#36573=CARTESIAN_POINT('Ctrl Pts',(-0.857646992606967,-1.29122544848478,
-0.628887879387163));
#36574=CARTESIAN_POINT('Ctrl Pts',(-0.786176409889718,-0.171433387447648,
-1.42596797677794));
#36575=CARTESIAN_POINT('Ctrl Pts',(-0.714705827172472,1.1053821595978,-0.917007098824021));
#36576=CARTESIAN_POINT('Ctrl Pts',(-0.643235244455224,1.36976900842759,
0.431821659129023));
#36577=CARTESIAN_POINT('Ctrl Pts',(-0.571764661737977,0.379625575419958,
1.38517192213728));
#36578=CARTESIAN_POINT('Ctrl Pts',(-0.500294079020729,-0.958274652820194,
1.06980712581625));
#36579=CARTESIAN_POINT('Ctrl Pts',(-0.428823496303483,-1.41838316065648,
-0.225300183736171));
#36580=CARTESIAN_POINT('Ctrl Pts',(-0.357352913586234,-0.579621661001341,
-1.31422083734243));
#36581=CARTESIAN_POINT('Ctrl Pts',(-0.285882330868989,0.790424325774726,
-1.19914371643322));
#36582=CARTESIAN_POINT('Ctrl Pts',(-0.21441174815174,1.43574007932854,0.0136277651574338));
#36583=CARTESIAN_POINT('Ctrl Pts',(-0.142941165434494,0.767580850576639,
1.21505288651533));
#36584=CARTESIAN_POINT('Ctrl Pts',(-0.0714705827172464,-0.606613081372982,
1.30138611697881));
#36585=CARTESIAN_POINT('Ctrl Pts',(-0.0238235275724144,-1.14778002846286,
0.567598962951908));
#36586=CARTESIAN_POINT('Ctrl Pts',(1.11022302462516E-15,-1.20342780657953,
0.167291704370495));
#36587=CARTESIAN_POINT('Ctrl Pts',(-7.8838231210763,0.655825660320174,-0.919496987602489));
#36588=CARTESIAN_POINT('Ctrl Pts',(-7.85999959350388,0.961686399426088,
-0.701343666934003));
#36589=CARTESIAN_POINT('Ctrl Pts',(-7.81235253835904,1.33331834053275,0.0603695630789417));
#36590=CARTESIAN_POINT('Ctrl Pts',(-7.74088195564181,0.670691182052459,
1.1554079629169));
#36591=CARTESIAN_POINT('Ctrl Pts',(-7.66941137292454,-0.606760686719055,
1.18877271873767));
#36592=CARTESIAN_POINT('Ctrl Pts',(-7.59794079020731,-1.32819903994816,
0.135081013648165));
#36593=CARTESIAN_POINT('Ctrl Pts',(-7.52647020749005,-0.833299368455494,
-1.04323337156808));
#36594=CARTESIAN_POINT('Ctrl Pts',(-7.45499962477282,0.424892711866708,
-1.26558294803777));
#36595=CARTESIAN_POINT('Ctrl Pts',(-7.38352904205555,1.29388673301154,-0.329043592414301));
#36596=CARTESIAN_POINT('Ctrl Pts',(-7.31205845933833,0.977840732709539,
0.908996131508284));
#36597=CARTESIAN_POINT('Ctrl Pts',(-7.24058787662107,-0.233814484914493,
1.31442319741893));
#36598=CARTESIAN_POINT('Ctrl Pts',(-7.16911729390383,-1.23131451482871,
0.51601556836383));
#36599=CARTESIAN_POINT('Ctrl Pts',(-7.09764671118657,-1.10106521969307,
-0.755026426267688));
#36600=CARTESIAN_POINT('Ctrl Pts',(-7.02617612846933,0.0376438692531656,
-1.3345347491804));
#36601=CARTESIAN_POINT('Ctrl Pts',(-6.95470554575208,1.14187430402945,-0.691757165391766));
#36602=CARTESIAN_POINT('Ctrl Pts',(-6.88323496303484,1.20027034679381,0.584598885225599));
#36603=CARTESIAN_POINT('Ctrl Pts',(-6.81176438031758,0.159346744189729,
1.32552333541284));
#36604=CARTESIAN_POINT('Ctrl Pts',(-6.74029379760034,-1.0275213207092,0.852410812968044));
#36605=CARTESIAN_POINT('Ctrl Pts',(-6.66882321488309,-1.27328970740752,
-0.401419351652376));
#36606=CARTESIAN_POINT('Ctrl Pts',(-6.59735263216585,-0.352860727310056,
-1.28759206219164));
#36607=CARTESIAN_POINT('Ctrl Pts',(-6.5258820494486,0.890750959441906,-0.994468127333838));
#36608=CARTESIAN_POINT('Ctrl Pts',(-6.45441146673135,1.31852994738913,0.209482420870793));
#36609=CARTESIAN_POINT('Ctrl Pts',(-6.38294088401411,0.538676373189495,
1.22156942150623));
#36610=CARTESIAN_POINT('Ctrl Pts',(-6.31147030129686,-0.734547202569097,
1.11482936417495));
#36611=CARTESIAN_POINT('Ctrl Pts',(-6.23999971857961,-1.33500402305489,
-0.0129752884426916));
#36612=CARTESIAN_POINT('Ctrl Pts',(-6.16852913586237,-0.712739792730926,
-1.12889595852926));
#36613=CARTESIAN_POINT('Ctrl Pts',(-6.09705855314511,0.562317936471494,
-1.21086854703574));
#36614=CARTESIAN_POINT('Ctrl Pts',(-6.02558797042787,1.32235251549876,-0.183814917318094));
#36615=CARTESIAN_POINT('Ctrl Pts',(-5.95411738771061,0.871253473580096,
1.01159353675267));
#36616=CARTESIAN_POINT('Ctrl Pts',(-5.88264680499337,-0.377820663234907,
1.28049039263217));
#36617=CARTESIAN_POINT('Ctrl Pts',(-5.81117622227613,-1.28085143983814,
0.376594859385609));
#36618=CARTESIAN_POINT('Ctrl Pts',(-5.73970563955887,-1.01075914682107,
-0.872221328647086));
#36619=CARTESIAN_POINT('Ctrl Pts',(-5.66823505684163,0.185080532705953,
-1.32217596994263));
#36620=CARTESIAN_POINT('Ctrl Pts',(-5.59676447412438,1.21140621873387,-0.561158687244707));
#36621=CARTESIAN_POINT('Ctrl Pts',(-5.52529389140713,1.12821323799053,0.713819997393794));
#36622=CARTESIAN_POINT('Ctrl Pts',(-5.45382330868989,0.0116974722997823,
1.33501583069457));
#36623=CARTESIAN_POINT('Ctrl Pts',(-5.38235272597264,-1.11553192823179,
0.733479799418535));
#36624=CARTESIAN_POINT('Ctrl Pts',(-5.3108821432554,-1.22105326865133,-0.539845361354251));
#36625=CARTESIAN_POINT('Ctrl Pts',(-5.23941156053815,-0.208220275292116,
-1.31872984952112));
#36626=CARTESIAN_POINT('Ctrl Pts',(-5.1679409778209,0.995320243473335,-0.889798691835582));
#36627=CARTESIAN_POINT('Ctrl Pts',(-5.09647039510366,1.28725376165656,0.354092999311268));
#36628=CARTESIAN_POINT('Ctrl Pts',(-5.0249998123864,0.400200367490025,1.27367333524777));
#36629=CARTESIAN_POINT('Ctrl Pts',(-4.95352922966917,-0.853393804915241,
1.02670497845901));
#36630=CARTESIAN_POINT('Ctrl Pts',(-4.8820586469519,-1.32537043069111,-0.16061544293722));
#36631=CARTESIAN_POINT('Ctrl Pts',(-4.81058806423467,-0.583449347759317,
-1.20082927914816));
#36632=CARTESIAN_POINT('Ctrl Pts',(-4.73911748151741,0.692849000570423,
-1.14121179518476));
#36633=CARTESIAN_POINT('Ctrl Pts',(-4.66764689880018,1.33457169005264,-0.0363662366802944));
#36634=CARTESIAN_POINT('Ctrl Pts',(-4.59617631608292,0.753969300337004,
1.10178690916601));
#36635=CARTESIAN_POINT('Ctrl Pts',(-4.52470573336568,-0.517188412570627,
1.23082096381356));
#36636=CARTESIAN_POINT('Ctrl Pts',(-4.45323515064843,-1.31465679723343,
0.232554519517921));
#36637=CARTESIAN_POINT('Ctrl Pts',(-4.38176456793118,-0.908040016765106,
-0.978707017964768));
#36638=CARTESIAN_POINT('Ctrl Pts',(-4.31029398521394,0.33024440185269,-1.29357749443364));
#36639=CARTESIAN_POINT('Ctrl Pts',(-4.23882340249668,1.26606023248978,-0.423669194971941));
#36640=CARTESIAN_POINT('Ctrl Pts',(-4.16735281977945,1.04230015912558,0.834274821235221));
#36641=CARTESIAN_POINT('Ctrl Pts',(-4.09588223706219,-0.136095498109634,
1.3281122371451));
#36642=CARTESIAN_POINT('Ctrl Pts',(-4.02441165434495,-1.18984221985096,
0.60554074257674));
#36643=CARTESIAN_POINT('Ctrl Pts',(-3.9529410716277,-1.15382059385002,-0.671641374743884));
#36644=CARTESIAN_POINT('Ctrl Pts',(-3.88147048891045,-0.0610225808853908,
-1.33367175259969));
#36645=CARTESIAN_POINT('Ctrl Pts',(-3.8099999061932,1.08766559636906,-0.774201297813038));
#36646=CARTESIAN_POINT('Ctrl Pts',(-3.73852932347596,1.24016829619131,0.494354828217767));
#36647=CARTESIAN_POINT('Ctrl Pts',(-3.66705874075871,0.256809339304101,
1.31013474967518));
#36648=CARTESIAN_POINT('Ctrl Pts',(-3.59558815804146,-0.961759534250261,
0.925971218418253));
#36649=CARTESIAN_POINT('Ctrl Pts',(-3.52411757532421,-1.29945943116285,
-0.306283015889169));
#36650=CARTESIAN_POINT('Ctrl Pts',(-3.45264699260697,-0.446993326541367,
-1.25801473166563));
#36651=CARTESIAN_POINT('Ctrl Pts',(-3.38117640988971,0.814870907336141,
-1.05753936259481));
#36652=CARTESIAN_POINT('Ctrl Pts',(-3.30970582717248,1.33040045288649,0.111529072531204));
#36653=CARTESIAN_POINT('Ctrl Pts',(-3.23823524445522,0.627425326818042,
1.17844879325643));
#36654=CARTESIAN_POINT('Ctrl Pts',(-3.16676466173798,-0.650204362965427,
1.16603532769852));
#36655=CARTESIAN_POINT('Ctrl Pts',(-3.09529407902073,-1.33231632569059,
0.0856580840236087));
#36656=CARTESIAN_POINT('Ctrl Pts',(-3.02382349630348,-0.794168882004904,
-1.07317281269857));
#36657=CARTESIAN_POINT('Ctrl Pts',(-2.95235291358624,0.47135240665934,-1.24909207338638));
#36658=CARTESIAN_POINT('Ctrl Pts',(-2.88088233086899,1.30516525126295,-0.280976450892185));
#36659=CARTESIAN_POINT('Ctrl Pts',(-2.80941174815174,0.943586172744538,
0.94448358041082));
#36660=CARTESIAN_POINT('Ctrl Pts',(-2.7379411654345,-0.282217024962677,
1.30489756298394));
#36661=CARTESIAN_POINT('Ctrl Pts',(-2.66647058271725,-1.24953958055837,
0.470164796298212));
#36662=CARTESIAN_POINT('Ctrl Pts',(-2.595,-1.0724173842155,-0.795188690244717));
#36663=CARTESIAN_POINT('Ctrl Pts',(-2.52352941728275,0.0869245563835385,
-1.33223429641986));
#36664=CARTESIAN_POINT('Ctrl Pts',(-2.45205883456551,1.1666528905657,-0.649095626232613));
#36665=CARTESIAN_POINT('Ctrl Pts',(-2.38058825184826,1.17785182502816,0.628545286627099));
#36666=CARTESIAN_POINT('Ctrl Pts',(-2.30911766913101,0.110264332319804,
1.33050587224349));
#36667=CARTESIAN_POINT('Ctrl Pts',(-2.23764708641377,-1.05831350787747,
0.813865233377982));
#36668=CARTESIAN_POINT('Ctrl Pts',(-2.16617650369651,-1.25758924766389,
-0.448189003926511));
#36669=CARTESIAN_POINT('Ctrl Pts',(-2.09470592097927,-0.305047600466661,
-1.29974999922249));
#36670=CARTESIAN_POINT('Ctrl Pts',(-2.02323533826202,0.926885056687137,
-0.960878863718607));
#36671=CARTESIAN_POINT('Ctrl Pts',(-1.95176475554478,1.30989003265289,0.25805464837349));
#36672=CARTESIAN_POINT('Ctrl Pts',(-1.88029417282753,0.493175690398631,
1.24063767362796));
#36673=CARTESIAN_POINT('Ctrl Pts',(-1.80882359011028,-0.775234891880261,
1.0869291428083));
#36674=CARTESIAN_POINT('Ctrl Pts',(-1.73735300739303,-1.33361314172858,
-0.0622903530799726));
#36675=CARTESIAN_POINT('Ctrl Pts',(-1.66588242467579,-0.670544239191035,
-1.15445854001498));
#36676=CARTESIAN_POINT('Ctrl Pts',(-1.59441184195854,0.606671541892842,
-1.18926605094919));
#36677=CARTESIAN_POINT('Ctrl Pts',(-1.52294125924129,1.32824101261299,-0.13483292046695));
#36678=CARTESIAN_POINT('Ctrl Pts',(-1.45147067652404,0.83328362117648,1.04309275391532));
#36679=CARTESIAN_POINT('Ctrl Pts',(-1.3800000938068,-0.424872523711829,
1.26565692247568));
#36680=CARTESIAN_POINT('Ctrl Pts',(-1.30852951108955,-1.2938908569106,0.329014556566575));
#36681=CARTESIAN_POINT('Ctrl Pts',(-1.23705892837231,-0.97784335900594,
-0.908969953708416));
#36682=CARTESIAN_POINT('Ctrl Pts',(-1.16558834565505,0.23380408827944,-1.31443517267865));
#36683=CARTESIAN_POINT('Ctrl Pts',(-1.09411776293781,1.23131214611387,-0.516018078568234));
#36684=CARTESIAN_POINT('Ctrl Pts',(-1.02264718022056,1.10106950189213,0.755016191621646));
#36685=CARTESIAN_POINT('Ctrl Pts',(-0.951176597503315,-0.0376345337404676,
1.33453677501585));
#36686=CARTESIAN_POINT('Ctrl Pts',(-0.879706014786067,-1.14187055595229,
0.691763352254813));
#36687=CARTESIAN_POINT('Ctrl Pts',(-0.808235432068821,-1.20027287402703,
-0.584589672793852));
#36688=CARTESIAN_POINT('Ctrl Pts',(-0.736764849351572,-0.159357798359248,
-1.32552427909955));
#36689=CARTESIAN_POINT('Ctrl Pts',(-0.665294266634327,1.02752019266317,
-0.852414074784762));
#36690=CARTESIAN_POINT('Ctrl Pts',(-0.593823683917078,1.27328390749102,
0.401404591644431));
#36691=CARTESIAN_POINT('Ctrl Pts',(-0.522353101199832,0.352885145656143,
1.28760185601691));
#36692=CARTESIAN_POINT('Ctrl Pts',(-0.450882518482584,-0.890774785299878,
0.994451027173357));
#36693=CARTESIAN_POINT('Ctrl Pts',(-0.379411935765338,-1.31847372951833,
-0.209430273674656));
#36694=CARTESIAN_POINT('Ctrl Pts',(-0.307941353048089,-0.538793715469893,
-1.22164849166681));
#36695=CARTESIAN_POINT('Ctrl Pts',(-0.236470770330843,0.734747660303497,
-1.11467728318377));
#36696=CARTESIAN_POINT('Ctrl Pts',(-0.165000187613595,1.33460804493414,
0.0126678395870271));
#36697=CARTESIAN_POINT('Ctrl Pts',(-0.0935296048963483,0.713513255683474,
1.129465827911));
#36698=CARTESIAN_POINT('Ctrl Pts',(-0.022059022179101,-0.563883888329778,
1.20971783562508));
#36699=CARTESIAN_POINT('Ctrl Pts',(0.0255880329657311,-1.06693159984617,
0.527617883737111));
#36700=CARTESIAN_POINT('Ctrl Pts',(0.0494115605381466,-1.11865960648645,
0.155507851120246));
#36701=CARTESIAN_POINT('Ctrl Pts',(-7.83441156053815,0.606129434160009,
-0.849820649797735));
#36702=CARTESIAN_POINT('Ctrl Pts',(-7.81058803296573,0.888813092246091,
-0.648198241866392));
#36703=CARTESIAN_POINT('Ctrl Pts',(-7.7629409778209,1.23228403552816,0.0557949640025797));
#36704=CARTESIAN_POINT('Ctrl Pts',(-7.69147039510365,0.619868497483138,
1.06785509802237));
#36705=CARTESIAN_POINT('Ctrl Pts',(-7.61999981238641,-0.560782436496941,
1.09869158672678));
#36706=CARTESIAN_POINT('Ctrl Pts',(-7.54852922966916,-1.22755265803812,
0.124845036298736));
#36707=CARTESIAN_POINT('Ctrl Pts',(-7.47705864695192,-0.770154791505453,
-0.964180713662061));
#36708=CARTESIAN_POINT('Ctrl Pts',(-7.40558806423467,0.39269579494153,-1.16968139947768));
#36709=CARTESIAN_POINT('Ctrl Pts',(-7.33411748151741,1.19584042040158,-0.304109794036846));
#36710=CARTESIAN_POINT('Ctrl Pts',(-7.26264689880018,0.903743305387708,
0.840115512674159));
#36711=CARTESIAN_POINT('Ctrl Pts',(-7.19117631608292,-0.216096822698968,
1.21482070175382));
#36712=CARTESIAN_POINT('Ctrl Pts',(-7.11970573336568,-1.13800971096765,
0.476913672937739));
#36713=CARTESIAN_POINT('Ctrl Pts',(-7.04823515064842,-1.017630262073,-0.697813105248224));
#36714=CARTESIAN_POINT('Ctrl Pts',(-6.97676456793119,0.0347913455519308,
-1.2334082688876));
#36715=CARTESIAN_POINT('Ctrl Pts',(-6.90529398521393,1.05534697353154,-0.639338172633152));
#36716=CARTESIAN_POINT('Ctrl Pts',(-6.83382340249669,1.10931796384116,0.540299980545708));
#36717=CARTESIAN_POINT('Ctrl Pts',(-6.76235281977944,0.147271992748498,
1.2250797092438));
#36718=CARTESIAN_POINT('Ctrl Pts',(-6.69088223706219,-0.949659268295102,
0.787818036098102));
#36719=CARTESIAN_POINT('Ctrl Pts',(-6.61941165434494,-1.17680416697311,
-0.371001165704848));
#36720=CARTESIAN_POINT('Ctrl Pts',(-6.5479410716277,-0.326122147885015,
-1.19002273821386));
#36721=CARTESIAN_POINT('Ctrl Pts',(-6.47647048891045,0.823252897363641,
-0.91911073289925));
#36722=CARTESIAN_POINT('Ctrl Pts',(-6.40499990619321,1.21861625625295,0.193608559273054));
#36723=CARTESIAN_POINT('Ctrl Pts',(-6.33352932347596,0.497857319454841,
1.12900306749702));
#36724=CARTESIAN_POINT('Ctrl Pts',(-6.26205874075871,-0.678885727099582,
1.03035140674798));
#36725=CARTESIAN_POINT('Ctrl Pts',(-6.19058815804147,-1.23384198279241,
-0.0119920654492216));
#36726=CARTESIAN_POINT('Ctrl Pts',(-6.11911757532421,-0.658730808215703,
-1.0433520826782));
#36727=CARTESIAN_POINT('Ctrl Pts',(-6.04764699260697,0.519707405905856,
-1.1191130687058));
#36728=CARTESIAN_POINT('Ctrl Pts',(-5.97617640988972,1.22214916322125,-0.169886051378017));
#36729=CARTESIAN_POINT('Ctrl Pts',(-5.90470582717248,0.805232864315218,
0.934938437347007));
#36730=CARTESIAN_POINT('Ctrl Pts',(-5.83323524445522,-0.349190705207747,
1.1834592088918));
#36731=CARTESIAN_POINT('Ctrl Pts',(-5.76176466173799,-1.18379289717498,
0.348057788582894));
#36732=CARTESIAN_POINT('Ctrl Pts',(-5.69029407902073,-0.934167274631489,
-0.806127378634508));
#36733=CARTESIAN_POINT('Ctrl Pts',(-5.61882349630348,0.171055762759161,
-1.22198599568372));
#36734=CARTESIAN_POINT('Ctrl Pts',(-5.54735291358624,1.11960999748104,-0.518636000621784));
#36735=CARTESIAN_POINT('Ctrl Pts',(-5.47588233086899,1.04272109636754,0.659729158662641));
#36736=CARTESIAN_POINT('Ctrl Pts',(-5.40441174815175,0.0108110778445307,
1.23385289568953));
#36737=CARTESIAN_POINT('Ctrl Pts',(-5.3329411654345,-1.03100073290279,0.677899208110117));
#36738=CARTESIAN_POINT('Ctrl Pts',(-5.26147058271725,-1.12852602694064,
-0.498937725693461));
#36739=CARTESIAN_POINT('Ctrl Pts',(-5.19,-0.192442054770818,-1.21880101048488));
#36740=CARTESIAN_POINT('Ctrl Pts',(-5.11852941728275,0.919898278591243,
-0.822372789340543));
#36741=CARTESIAN_POINT('Ctrl Pts',(-5.04705883456551,1.18971007293662,0.327261042527343));
#36742=CARTESIAN_POINT('Ctrl Pts',(-4.97558825184826,0.369874551994385,
1.17715872480732));
#36743=CARTESIAN_POINT('Ctrl Pts',(-4.90411766913101,-0.788726540276575,
0.948904785669409));
#36744=CARTESIAN_POINT('Ctrl Pts',(-4.83264708641377,-1.22493839111908,
-0.148444553842822));
#36745=CARTESIAN_POINT('Ctrl Pts',(-4.76117650369652,-0.539237551098138,
-1.10983454221279));
#36746=CARTESIAN_POINT('Ctrl Pts',(-4.68970592097927,0.640347272275161,
-1.05473466734186));
#36747=CARTESIAN_POINT('Ctrl Pts',(-4.61823533826202,1.23344241050686,-0.0336105276069657));
#36748=CARTESIAN_POINT('Ctrl Pts',(-4.54676475554478,0.696836084706056,
1.01829726438527));
#36749=CARTESIAN_POINT('Ctrl Pts',(-4.47529417282753,-0.47799764302072,
1.13755355956088));
#36750=CARTESIAN_POINT('Ctrl Pts',(-4.40382359011028,-1.21503660017309,
0.214932333172088));
#36751=CARTESIAN_POINT('Ctrl Pts',(-4.33235300739304,-0.839231849037084,
-0.904543946508284));
#36752=CARTESIAN_POINT('Ctrl Pts',(-4.26088242467578,0.305219610241788,
-1.19555461486577));
#36753=CARTESIAN_POINT('Ctrl Pts',(-4.18941184195855,1.17012251694585,-0.391564991973613));
#36754=CARTESIAN_POINT('Ctrl Pts',(-4.11794125924129,0.963318216867623,
0.771056327808787));
#36755=CARTESIAN_POINT('Ctrl Pts',(-4.04647067652406,-0.125782646596431,
1.22747243285468));
#36756=CARTESIAN_POINT('Ctrl Pts',(-3.97500009380679,-1.09968004470252,
0.559654935550513));
#36757=CARTESIAN_POINT('Ctrl Pts',(-3.90352951108956,-1.06638801435588,
-0.620746687821297));
#36758=CARTESIAN_POINT('Ctrl Pts',(-3.8320589283723,-0.0563984983524121,
-1.23261066723705));
#36759=CARTESIAN_POINT('Ctrl Pts',(-3.76058834565506,1.00524601638892,-0.715534970589979));
#36760=CARTESIAN_POINT('Ctrl Pts',(-3.68911776293781,1.14619258305115,0.456894309618231));
#36761=CARTESIAN_POINT('Ctrl Pts',(-3.61764718022056,0.237349205646206,
1.21085721791717));
#36762=CARTESIAN_POINT('Ctrl Pts',(-3.54617659750332,-0.888880685163351,
0.855804285538767));
#36763=CARTESIAN_POINT('Ctrl Pts',(-3.47470601478607,-1.20099083854098,
-0.283073936178549));
#36764=CARTESIAN_POINT('Ctrl Pts',(-3.40323543206882,-0.41312170060186,
-1.16268667666522));
#36765=CARTESIAN_POINT('Ctrl Pts',(-3.33176484935158,0.753122776159715,
-0.977402645603371));
#36766=CARTESIAN_POINT('Ctrl Pts',(-3.26029426663433,1.22958725543099,0.103077780751569));
#36767=CARTESIAN_POINT('Ctrl Pts',(-3.18882368391708,0.579881180825104,
1.08914997301927));
#36768=CARTESIAN_POINT('Ctrl Pts',(-3.11735310119984,-0.60093409949864,
1.07767715743758));
#36769=CARTESIAN_POINT('Ctrl Pts',(-3.04588251848258,-1.23135794994468,
0.0791672072957683));
#36770=CARTESIAN_POINT('Ctrl Pts',(-2.97441193576534,-0.733989479524334,
-0.991851446311691));
#36771=CARTESIAN_POINT('Ctrl Pts',(-2.90294135304809,0.435634932916331,
-1.15444014692229));
#36772=CARTESIAN_POINT('Ctrl Pts',(-2.83147077033084,1.20626429110306,-0.259685016149587));
#36773=CARTESIAN_POINT('Ctrl Pts',(-2.7600001876136,0.872084438854716,0.872913844036455));
#36774=CARTESIAN_POINT('Ctrl Pts',(-2.68852960489635,-0.260831583758772,
1.20601688732655));
#36775=CARTESIAN_POINT('Ctrl Pts',(-2.61705902217911,-1.1548537435309,0.434537315607708));
#36776=CARTESIAN_POINT('Ctrl Pts',(-2.54558843946186,-0.991153261616114,
-0.734932010182651));
#36777=CARTESIAN_POINT('Ctrl Pts',(-2.47411785674461,0.08033771071057,-1.23128213657162));
#36778=CARTESIAN_POINT('Ctrl Pts',(-2.40264727402736,1.07824792350225,-0.599909379044461));
#36779=CARTESIAN_POINT('Ctrl Pts',(-2.33117669131011,1.08859824100219,0.580916273909186));
#36780=CARTESIAN_POINT('Ctrl Pts',(-2.25970610859287,0.101908878229005,
1.22968468646956));
#36781=CARTESIAN_POINT('Ctrl Pts',(-2.18823552587562,-0.978118128803457,
0.752193308735518));
#36782=CARTESIAN_POINT('Ctrl Pts',(-2.11676494315837,-1.16229343438632,
-0.414226773643003));
#36783=CARTESIAN_POINT('Ctrl Pts',(-2.04529436044113,-0.281932136312642,
-1.20125938834656));
#36784=CARTESIAN_POINT('Ctrl Pts',(-1.97382377772388,0.856648876268221,
-0.888066748833407));
#36785=CARTESIAN_POINT('Ctrl Pts',(-1.90235319500663,1.21063104471409,0.238500149452261));
#36786=CARTESIAN_POINT('Ctrl Pts',(-1.83088261228938,0.455804522831336,
1.14662639267054));
#36787=CARTESIAN_POINT('Ctrl Pts',(-1.75941202957214,-0.71649024243284,
1.00456536876091));
#36788=CARTESIAN_POINT('Ctrl Pts',(-1.68794144685489,-1.23255649769735,
-0.0575702031048387));
#36789=CARTESIAN_POINT('Ctrl Pts',(-1.61647086413764,-0.61973268944933,
-1.06697761914173));
#36790=CARTESIAN_POINT('Ctrl Pts',(-1.54500028142039,0.560700046760855,
-1.09914753591009));
#36791=CARTESIAN_POINT('Ctrl Pts',(-1.47352969870315,1.22759145015792,-0.124615742770522));
#36792=CARTESIAN_POINT('Ctrl Pts',(-1.4020591159859,0.7701402375014,0.964050751534233));
#36793=CARTESIAN_POINT('Ctrl Pts',(-1.33058853326865,-0.392677136576001,
1.16974976838562));
#36794=CARTESIAN_POINT('Ctrl Pts',(-1.2591179505514,-1.19584423180567,0.304082958426382));
#36795=CARTESIAN_POINT('Ctrl Pts',(-1.18764736783416,-0.903745732672346,
-0.840091318538458));
#36796=CARTESIAN_POINT('Ctrl Pts',(-1.11617678511691,0.216087213885371,
-1.21483176956931));
#36797=CARTESIAN_POINT('Ctrl Pts',(-1.04470620239966,1.13800752174592,-0.476915992927436));
#36798=CARTESIAN_POINT('Ctrl Pts',(-0.973235619682416,1.01763421978166,
0.697803646148666));
#36799=CARTESIAN_POINT('Ctrl Pts',(-0.90176503696517,-0.0347827174524657,
1.23341014121216));
#36800=CARTESIAN_POINT('Ctrl Pts',(-0.830294454247921,-1.05534350947085,
0.639343890676872));
#36801=CARTESIAN_POINT('Ctrl Pts',(-0.758823871530676,-1.10932029956929,
-0.540291466200541));
#36802=CARTESIAN_POINT('Ctrl Pts',(-0.687353288813426,-0.147282209270845,
-1.22508058142116));
#36803=CARTESIAN_POINT('Ctrl Pts',(-0.615882706096181,0.949658225728546,
-0.787821050745502));
#36804=CARTESIAN_POINT('Ctrl Pts',(-0.544412123378933,1.17679880655445,
0.370987524159838));
#36805=CARTESIAN_POINT('Ctrl Pts',(-0.472941540661687,0.326144715892325,
1.19003178989654));
#36806=CARTESIAN_POINT('Ctrl Pts',(-0.401470957944438,-0.823274917779561,
0.919094928530463));
#36807=CARTESIAN_POINT('Ctrl Pts',(-0.330000375227192,-1.21856429838018,
-0.193560363613141));
#36808=CARTESIAN_POINT('Ctrl Pts',(-0.258529792509943,-0.497965769938443,
-1.12907614599118));
#36809=CARTESIAN_POINT('Ctrl Pts',(-0.187059209792698,0.679070994832269,
-1.03021084993432));
#36810=CARTESIAN_POINT('Ctrl Pts',(-0.11558862707545,1.23347601053973,0.0117079140166205));
#36811=CARTESIAN_POINT('Ctrl Pts',(-0.0441180443582029,0.659445660790309,
1.04387876930667));
#36812=CARTESIAN_POINT('Ctrl Pts',(0.0273525383590445,-0.521154695286574,
1.11804955427136));
#36813=CARTESIAN_POINT('Ctrl Pts',(0.0749995935038766,-0.986083171229488,
0.487636804522315));
#36814=CARTESIAN_POINT('Ctrl Pts',(0.098823121076292,-1.03389140639336,
0.143723997869997));
#36815=CARTESIAN_POINT('Ctrl Pts',(-7.785,0.556433207999845,-0.780144311992981));
#36816=CARTESIAN_POINT('Ctrl Pts',(-7.76117647242759,0.815939785066093,
-0.595052816798781));
#36817=CARTESIAN_POINT('Ctrl Pts',(-7.71352941728275,1.13124973052358,0.0512203649262202));
#36818=CARTESIAN_POINT('Ctrl Pts',(-7.64205883456552,0.569045812913815,
0.980302233127841));
#36819=CARTESIAN_POINT('Ctrl Pts',(-7.57058825184826,-0.514804186274824,
1.00861045471588));
#36820=CARTESIAN_POINT('Ctrl Pts',(-7.49911766913102,-1.12690627612808,
0.114609058949306));
#36821=CARTESIAN_POINT('Ctrl Pts',(-7.42764708641376,-0.70701021455541,
-0.88512805575604));
#36822=CARTESIAN_POINT('Ctrl Pts',(-7.35617650369652,0.360498878016349,
-1.07377985091759));
#36823=CARTESIAN_POINT('Ctrl Pts',(-7.28470592097927,1.09779410779162,-0.279175995659392));
#36824=CARTESIAN_POINT('Ctrl Pts',(-7.21323533826203,0.829645878065874,
0.771234893840035));
#36825=CARTESIAN_POINT('Ctrl Pts',(-7.14176475554478,-0.198379160483441,
1.11521820608871));
#36826=CARTESIAN_POINT('Ctrl Pts',(-7.07029417282753,-1.04470490710658,
0.43781177751165));
#36827=CARTESIAN_POINT('Ctrl Pts',(-6.99882359011028,-0.93419530445292,
-0.640599784228763));
#36828=CARTESIAN_POINT('Ctrl Pts',(-6.92735300739304,0.0319388218506953,
-1.1322817885948));
#36829=CARTESIAN_POINT('Ctrl Pts',(-6.85588242467578,0.968819643033635,
-0.586919179874541));
#36830=CARTESIAN_POINT('Ctrl Pts',(-6.78441184195855,1.0183655808885,0.496001075865819));
#36831=CARTESIAN_POINT('Ctrl Pts',(-6.71294125924129,0.135197241307266,
1.12463608307476));
#36832=CARTESIAN_POINT('Ctrl Pts',(-6.64147067652406,-0.871797215881005,
0.723225259228162));
#36833=CARTESIAN_POINT('Ctrl Pts',(-6.57000009380679,-1.0803186265387,-0.340582979757321));
#36834=CARTESIAN_POINT('Ctrl Pts',(-6.49852951108958,-0.299383568459973,
-1.09245341423609));
#36835=CARTESIAN_POINT('Ctrl Pts',(-6.42705892837228,0.755754835285377,
-0.843753338464662));
#36836=CARTESIAN_POINT('Ctrl Pts',(-6.35558834565508,1.11870256511677,0.177734697675315));
#36837=CARTESIAN_POINT('Ctrl Pts',(-6.28411776293779,0.457038265720188,
1.03643671348781));
#36838=CARTESIAN_POINT('Ctrl Pts',(-6.21264718022058,-0.623224251630068,
0.945873449321006));
#36839=CARTESIAN_POINT('Ctrl Pts',(-6.14117659750331,-1.13267994252993,
-0.0110088424557517));
#36840=CARTESIAN_POINT('Ctrl Pts',(-6.06970601478608,-0.604721823700482,
-0.957808206827138));
#36841=CARTESIAN_POINT('Ctrl Pts',(-5.99823543206882,0.47709687534022,-1.02735759037585));
#36842=CARTESIAN_POINT('Ctrl Pts',(-5.92676484935158,1.12194581094373,-0.155957185437944));
#36843=CARTESIAN_POINT('Ctrl Pts',(-5.85529426663432,0.739212255050342,
0.858283337941351));
#36844=CARTESIAN_POINT('Ctrl Pts',(-5.78382368391709,-0.320560747180587,
1.08642802515142));
#36845=CARTESIAN_POINT('Ctrl Pts',(-5.71235310119983,-1.08673435451183,
0.319520717780182));
#36846=CARTESIAN_POINT('Ctrl Pts',(-5.64088251848259,-0.857575402441912,
-0.740033428621935));
#36847=CARTESIAN_POINT('Ctrl Pts',(-5.56941193576534,0.157030992812372,
-1.1217960214248));
#36848=CARTESIAN_POINT('Ctrl Pts',(-5.49794135304809,1.02781377622821,-0.476113313998863));
#36849=CARTESIAN_POINT('Ctrl Pts',(-5.42647077033084,0.957228954744552,
0.605638319931491));
#36850=CARTESIAN_POINT('Ctrl Pts',(-5.3550001876136,0.00992468338927851,
1.13268996068449));
#36851=CARTESIAN_POINT('Ctrl Pts',(-5.28352960489635,-0.946469537573792,
0.6223186168017));
#36852=CARTESIAN_POINT('Ctrl Pts',(-5.21205902217911,-1.03599878522995,
-0.458030090032672));
#36853=CARTESIAN_POINT('Ctrl Pts',(-5.14058843946185,-0.176663834249519,
-1.11887217144864));
#36854=CARTESIAN_POINT('Ctrl Pts',(-5.06911785674461,0.844476313709149,
-0.754946886845504));
#36855=CARTESIAN_POINT('Ctrl Pts',(-4.99764727402736,1.09216638421668,0.30042908574342));
#36856=CARTESIAN_POINT('Ctrl Pts',(-4.92617669131012,0.339548736498745,
1.08064411436687));
#36857=CARTESIAN_POINT('Ctrl Pts',(-4.85470610859287,-0.72405927563791,
0.871104592879805));
#36858=CARTESIAN_POINT('Ctrl Pts',(-4.78323552587562,-1.12450635154704,
-0.136273664748425));
#36859=CARTESIAN_POINT('Ctrl Pts',(-4.71176494315838,-0.495025754436958,
-1.01883980527742));
#36860=CARTESIAN_POINT('Ctrl Pts',(-4.64029436044113,0.587845543979899,
-0.968257539498959));
#36861=CARTESIAN_POINT('Ctrl Pts',(-4.56882377772388,1.13231313096107,-0.0308548185336372));
#36862=CARTESIAN_POINT('Ctrl Pts',(-4.49735319500663,0.639702869075108,
0.934807619604525));
#36863=CARTESIAN_POINT('Ctrl Pts',(-4.42588261228939,-0.438806873470812,
1.0442861553082));
#36864=CARTESIAN_POINT('Ctrl Pts',(-4.35441202957213,-1.11541640311276,
0.197310146826257));
#36865=CARTESIAN_POINT('Ctrl Pts',(-4.2829414468549,-0.770423681309061,
-0.830380875051803));
#36866=CARTESIAN_POINT('Ctrl Pts',(-4.21147086413764,0.280194818630884,
-1.09753173529789));
#36867=CARTESIAN_POINT('Ctrl Pts',(-4.1400002814204,1.07418480140191,-0.359460788975286));
#36868=CARTESIAN_POINT('Ctrl Pts',(-4.06852969870314,0.884336274609667,
0.707837834382355));
#36869=CARTESIAN_POINT('Ctrl Pts',(-3.99705911598591,-0.115469795083229,
1.12683262856426));
#36870=CARTESIAN_POINT('Ctrl Pts',(-3.92558853326865,-1.00951786955407,
0.513769128524286));
#36871=CARTESIAN_POINT('Ctrl Pts',(-3.85411795055141,-0.978955434861744,
-0.569852000898709));
#36872=CARTESIAN_POINT('Ctrl Pts',(-3.78264736783416,-0.0517744158194337,
-1.13154958187441));
#36873=CARTESIAN_POINT('Ctrl Pts',(-3.71117678511691,0.922826436408769,
-0.65686864336692));
#36874=CARTESIAN_POINT('Ctrl Pts',(-3.63970620239967,1.05221686991099,0.419433791018696));
#36875=CARTESIAN_POINT('Ctrl Pts',(-3.56823561968242,0.217889071988309,
1.11157968615915));
#36876=CARTESIAN_POINT('Ctrl Pts',(-3.49676503696517,-0.816001836076439,
0.785637352659282));
#36877=CARTESIAN_POINT('Ctrl Pts',(-3.42529445424792,-1.1025222459191,-0.25986485646793));
#36878=CARTESIAN_POINT('Ctrl Pts',(-3.35382387153068,-0.379250074662353,
-1.06735862166481));
#36879=CARTESIAN_POINT('Ctrl Pts',(-3.28235328881343,0.69137464498329,-0.897265928611934));
#36880=CARTESIAN_POINT('Ctrl Pts',(-3.21088270609618,1.12877405797548,0.0946264889719359));
#36881=CARTESIAN_POINT('Ctrl Pts',(-3.13941212337894,0.532337034832168,
0.999851152782103));
#36882=CARTESIAN_POINT('Ctrl Pts',(-3.06794154066169,-0.551663836031854,
0.989318987176647));
#36883=CARTESIAN_POINT('Ctrl Pts',(-2.99647095794444,-1.13039957419878,
0.0726763305679285));
#36884=CARTESIAN_POINT('Ctrl Pts',(-2.92500037522719,-0.673810077043764,
-0.910530079924814));
#36885=CARTESIAN_POINT('Ctrl Pts',(-2.85352979250995,0.399917459173323,
-1.05978822045819));
#36886=CARTESIAN_POINT('Ctrl Pts',(-2.78205920979269,1.10736333094316,-0.238393581406989));
#36887=CARTESIAN_POINT('Ctrl Pts',(-2.71058862707545,0.800582704964894,
0.801344107662086));
#36888=CARTESIAN_POINT('Ctrl Pts',(-2.6391180443582,-0.239446142554869,
1.10713621166916));
#36889=CARTESIAN_POINT('Ctrl Pts',(-2.56764746164096,-1.06016790650342,
0.398909834917203));
#36890=CARTESIAN_POINT('Ctrl Pts',(-2.49617687892371,-0.909889139016734,
-0.674675330120583));
#36891=CARTESIAN_POINT('Ctrl Pts',(-2.42470629620646,0.0737508650376029,
-1.13032997672338));
#36892=CARTESIAN_POINT('Ctrl Pts',(-2.35323571348922,0.989842956438803,
-0.550723131856308));
#36893=CARTESIAN_POINT('Ctrl Pts',(-2.28176513077197,0.999344656976215,
0.533287261191272));
#36894=CARTESIAN_POINT('Ctrl Pts',(-2.21029454805472,0.0935534241382057,
1.12886350069563));
#36895=CARTESIAN_POINT('Ctrl Pts',(-2.13882396533747,-0.897922749729446,
0.690521384093054));
#36896=CARTESIAN_POINT('Ctrl Pts',(-2.06735338262023,-1.06699762110876,
-0.380264543359496));
#36897=CARTESIAN_POINT('Ctrl Pts',(-1.99588279990298,-0.258816672158623,
-1.10276877747064));
#36898=CARTESIAN_POINT('Ctrl Pts',(-1.92441221718573,0.786412695849304,
-0.815254633948207));
#36899=CARTESIAN_POINT('Ctrl Pts',(-1.85294163446849,1.11137205677529,0.218945650531032));
#36900=CARTESIAN_POINT('Ctrl Pts',(-1.78147105175124,0.418433355264041,
1.05261511171313));
#36901=CARTESIAN_POINT('Ctrl Pts',(-1.71000046903399,-0.657745592985418,
0.922201594713525));
#36902=CARTESIAN_POINT('Ctrl Pts',(-1.63852988631674,-1.13149985366612,
-0.0528500531297068));
#36903=CARTESIAN_POINT('Ctrl Pts',(-1.5670593035995,-0.568921139707624,
-0.979496698268463));
#36904=CARTESIAN_POINT('Ctrl Pts',(-1.49558872088225,0.514728551628869,
-1.00902902087099));
#36905=CARTESIAN_POINT('Ctrl Pts',(-1.424118138165,1.12694188770285,-0.114398565074092));
#36906=CARTESIAN_POINT('Ctrl Pts',(-1.35264755544776,0.706996853826318,
0.885008749153142));
#36907=CARTESIAN_POINT('Ctrl Pts',(-1.28117697273051,-0.360481749440169,
1.07384261429556));
#36908=CARTESIAN_POINT('Ctrl Pts',(-1.20970639001326,-1.09779760670074,
0.279151360286191));
#36909=CARTESIAN_POINT('Ctrl Pts',(-1.13823580729601,-0.82964810633875,
-0.771212683368502));
#36910=CARTESIAN_POINT('Ctrl Pts',(-1.06676522457877,0.1983703394913,-1.11522836645996));
#36911=CARTESIAN_POINT('Ctrl Pts',(-0.995294641861518,1.04470289737796,
-0.437813907286639));
#36912=CARTESIAN_POINT('Ctrl Pts',(-0.923824059144271,0.934198937671177,
0.640591100675686));
#36913=CARTESIAN_POINT('Ctrl Pts',(-0.852353476427024,-0.0319309011644629,
1.13228350740848));
#36914=CARTESIAN_POINT('Ctrl Pts',(-0.780882893709776,-0.968816462989413,
0.586924429098932));
#36915=CARTESIAN_POINT('Ctrl Pts',(-0.709412310992529,-1.01836772511154,
-0.49599325960723));
#36916=CARTESIAN_POINT('Ctrl Pts',(-0.637941728275282,-0.135206620182443,
-1.12463688374277));
#36917=CARTESIAN_POINT('Ctrl Pts',(-0.566471145558034,0.87179625879392,
-0.723228026706244));
#36918=CARTESIAN_POINT('Ctrl Pts',(-0.495000562840788,1.08031370561788,
0.340570456675246));
#36919=CARTESIAN_POINT('Ctrl Pts',(-0.42352998012354,0.299404286128507,
1.09246172377618));
#36920=CARTESIAN_POINT('Ctrl Pts',(-0.352059397406293,-0.755775050259243,
0.843738829887568));
#36921=CARTESIAN_POINT('Ctrl Pts',(-0.280588814689047,-1.11865486724203,
-0.177690453551626));
#36922=CARTESIAN_POINT('Ctrl Pts',(-0.209118231971798,-0.457137824406994,
-1.03650380031556));
#36923=CARTESIAN_POINT('Ctrl Pts',(-0.137647649254552,0.62339432936104,
-0.945744416684868));
#36924=CARTESIAN_POINT('Ctrl Pts',(-0.0661770665373043,1.13234397614533,
0.0107479884462148));
#36925=CARTESIAN_POINT('Ctrl Pts',(0.00529351617994261,0.605378065897145,
0.958291710702337));
#36926=CARTESIAN_POINT('Ctrl Pts',(0.07676409889719,-0.478425502243371,
1.02638127291764));
#36927=CARTESIAN_POINT('Ctrl Pts',(0.124411154042022,-0.905234742612801,
0.447655725307518));
#36928=CARTESIAN_POINT('Ctrl Pts',(0.148234681614438,-0.949123206300278,
0.131940144619747));
#36929=CARTESIAN_POINT('Ctrl Pts',(-1.11022302462516E-16,0.570663374910274,
0.771750967939225));
#36930=CARTESIAN_POINT('Ctrl Pts',(-1.6227853268113E-16,0.553554149972714,
0.78839235193671));
#36931=CARTESIAN_POINT('Ctrl Pts',(-1.23639223896832E-15,0.535816051891995,
0.804318657007652));
#36932=CARTESIAN_POINT('Ctrl Pts',(-5.55111512312578E-16,0.517476131545855,
0.819482603444016));
#36933=CARTESIAN_POINT('Ctrl Pts',(6.73446525316235E-16,0.484403631959195,
0.846827848286062));
#36934=CARTESIAN_POINT('Ctrl Pts',(1.46277561945344E-15,0.449377049094155,
0.871696546385583));
#36935=CARTESIAN_POINT('Ctrl Pts',(1.88737914186277E-15,0.412720708654321,
0.894110857505424));
#36936=CARTESIAN_POINT('Ctrl Pts',(2.02722893480718E-15,0.400647371175813,
0.901493360484473));
#36937=CARTESIAN_POINT('Ctrl Pts',(1.96982266612964E-15,0.388396839386775,
0.908609315816784));
#36938=CARTESIAN_POINT('Ctrl Pts',(1.85962356624714E-15,0.375979633652141,
0.915458615713178));
#36939=CARTESIAN_POINT('Ctrl Pts',(1.76000123446738E-15,0.364754215379286,
0.921650528600536));
#36940=CARTESIAN_POINT('Ctrl Pts',(2.82869925563963E-15,0.353389819517391,
0.9276256539064));
#36941=CARTESIAN_POINT('Ctrl Pts',(2.72004641033163E-15,0.341916629859017,
0.933372903137718));
#36942=CARTESIAN_POINT('Ctrl Pts',(2.35276881084968E-15,0.303133977235575,
0.952800244366746));
#36943=CARTESIAN_POINT('Ctrl Pts',(1.1688040584756E-15,0.263061982855837,
0.969655391781731));
#36944=CARTESIAN_POINT('Ctrl Pts',(2.08166817117217E-15,0.222016046761304,
0.983957630079311));
#36945=CARTESIAN_POINT('Ctrl Pts',(2.69006659399074E-15,0.194660077306816,
0.993489672255138));
#36946=CARTESIAN_POINT('Ctrl Pts',(1.53826374099029E-15,0.166870521404496,
1.00188706363919));
#36947=CARTESIAN_POINT('Ctrl Pts',(1.38777878078145E-15,0.138732201281755,
1.0091461379835));
#36948=CARTESIAN_POINT('Ctrl Pts',(1.33800608025447E-15,0.129425489309623,
1.01154706717231));
#36949=CARTESIAN_POINT('Ctrl Pts',(2.68620275761292E-15,0.120080580177726,
1.01382340557925));
#36950=CARTESIAN_POINT('Ctrl Pts',(2.692290834716E-15,0.110700425114071,
1.01597482323229));
#36951=CARTESIAN_POINT('Ctrl Pts',(2.6983819628624E-15,0.101315569180366,
1.01812731906951));
#36952=CARTESIAN_POINT('Ctrl Pts',(3.01944477006372E-15,0.0919037451979173,
1.02015282977562));
#36953=CARTESIAN_POINT('Ctrl Pts',(2.95596880306448E-15,0.08247156602505,
1.02205097598145));
#36954=CARTESIAN_POINT('Ctrl Pts',(2.65201403921594E-15,0.037305561809622,
1.03114025195497));
#36955=CARTESIAN_POINT('Ctrl Pts',(3.06257071685217E-15,-0.00834860240433294,
1.03731815327265));
#36956=CARTESIAN_POINT('Ctrl Pts',(3.10862446895044E-15,-0.0541501896412871,
1.04060058451353));
#36957=CARTESIAN_POINT('Ctrl Pts',(3.15460360551374E-15,-0.0998775698966539,
1.04387769761306));
#36958=CARTESIAN_POINT('Ctrl Pts',(3.03885975298288E-15,-0.145753160502293,
1.0442690927114));
#36959=CARTESIAN_POINT('Ctrl Pts',(3.48332473976143E-15,-0.191464036720484,
1.0417442192531));
#36960=CARTESIAN_POINT('Ctrl Pts',(3.70609819577921E-15,-0.214375109978547,
1.04047870947608));
#36961=CARTESIAN_POINT('Ctrl Pts',(1.06235067126326E-15,-0.237245096712249,
1.03847981622708));
#36962=CARTESIAN_POINT('Ctrl Pts',(9.0205620750794E-16,-0.260035528443775,
1.03573883777575));
#36963=CARTESIAN_POINT('Ctrl Pts',(8.33206419365417E-16,-0.269824490330739,
1.03456153082917));
#36964=CARTESIAN_POINT('Ctrl Pts',(8.13320907073322E-16,-0.279598777118199,
1.03324727556146));
#36965=CARTESIAN_POINT('Ctrl Pts',(7.63278329429795E-16,-0.289355335937033,
1.03179518646881));
#36966=CARTESIAN_POINT('Ctrl Pts',(7.23513230033157E-16,-0.297108144634533,
1.03064131970532));
#36967=CARTESIAN_POINT('Ctrl Pts',(1.46426492949664E-15,-0.304847930595704,
1.02940061940942));
#36968=CARTESIAN_POINT('Ctrl Pts',(1.4432899320127E-15,-0.312563996860672,
1.02807450029725));
#36969=CARTESIAN_POINT('Ctrl Pts',(1.31665470348709E-15,-0.359149261794851,
1.02006813953604));
#36970=CARTESIAN_POINT('Ctrl Pts',(-6.4851176683571E-16,-0.404962145828001,
1.00893866567721));
#36971=CARTESIAN_POINT('Ctrl Pts',(-6.93889390390723E-16,-0.449670173943294,
0.994677276149143));
#36972=CARTESIAN_POINT('Ctrl Pts',(-6.97600981451806E-16,-0.45332699650277,
0.993510788313419));
#36973=CARTESIAN_POINT('Ctrl Pts',(1.49899777376848E-15,-0.456976434972893,
0.992323319606125));
#36974=CARTESIAN_POINT('Ctrl Pts',(1.51267887105178E-15,-0.460618310709277,
0.991114850128469));
#36975=CARTESIAN_POINT('Ctrl Pts',(1.67393459725224E-15,-0.503544203599426,
0.976870917849112));
#36976=CARTESIAN_POINT('Ctrl Pts',(1.12125522885397E-15,-0.545419935519386,
0.959713756948874));
#36977=CARTESIAN_POINT('Ctrl Pts',(7.49400541621981E-16,-0.58610720628139,
0.939888327104482));
#36978=CARTESIAN_POINT('Ctrl Pts',(5.63148709306203E-16,-0.606486346282988,
0.929958312069705));
#36979=CARTESIAN_POINT('Ctrl Pts',(1.00622254320331E-15,-0.626567238076758,
0.919358074802143));
#36980=CARTESIAN_POINT('Ctrl Pts',(8.67361737988404E-16,-0.646331465200864,
0.908113776412865));
#36981=CARTESIAN_POINT('Ctrl Pts',(7.95690601173239E-16,-0.656532505185225,
0.902310183044663));
#36982=CARTESIAN_POINT('Ctrl Pts',(-4.50726463038882E-16,-0.666649171563993,
0.896334966382544));
#36983=CARTESIAN_POINT('Ctrl Pts',(-4.30211422042248E-16,-0.676678817816388,
0.890191433267475));
#36984=CARTESIAN_POINT('Ctrl Pts',(-4.11809703290141E-16,-0.685675277026487,
0.884680765823705));
#36985=CARTESIAN_POINT('Ctrl Pts',(-7.31588621547825E-16,-0.694602965016621,
0.879033670020616));
#36986=CARTESIAN_POINT('Ctrl Pts',(-7.49400541621981E-16,-0.703442280964398,
0.873264474759485));
#36987=CARTESIAN_POINT('Ctrl Pts',(-8.29389137610011E-16,-0.743137298077302,
0.847356553154324));
#36988=CARTESIAN_POINT('Ctrl Pts',(4.14969713553736E-16,-0.781133291997709,
0.818941549086768));
#36989=CARTESIAN_POINT('Ctrl Pts',(2.35922392732846E-16,-0.817284769458134,
0.788303358144051));
#36990=CARTESIAN_POINT('Ctrl Pts',(5.28234168389171E-17,-0.854254317339153,
0.756971856733506));
#36991=CARTESIAN_POINT('Ctrl Pts',(1.57130807400593E-15,-0.889295824999286,
0.723314911167561));
#36992=CARTESIAN_POINT('Ctrl Pts',(1.68615121864946E-15,-0.922238196069141,
0.687583577395874));
#36993=CARTESIAN_POINT('Ctrl Pts',(1.74491354597361E-15,-0.939093972682094,
0.669300759232564));
#36994=CARTESIAN_POINT('Ctrl Pts',(1.80102997402413E-15,-0.955399840771159,
0.650474053122468));
#36995=CARTESIAN_POINT('Ctrl Pts',(1.98452365651747E-15,-0.971130158053256,
0.631132646543269));
#36996=CARTESIAN_POINT('Ctrl Pts',(2.11257469800354E-15,-0.982107557838951,
0.617635248580471));
#36997=CARTESIAN_POINT('Ctrl Pts',(7.30982271506299E-16,-0.992804626999012,
0.603887133573503));
#36998=CARTESIAN_POINT('Ctrl Pts',(6.52256026967279E-16,-1.00321195432393,
0.589897488249048));
#36999=CARTESIAN_POINT('Ctrl Pts',(6.10633372201704E-16,-1.00871432008283,
0.582501146901354));
#37000=CARTESIAN_POINT('Ctrl Pts',(1.17225784430234E-15,-1.0141354010843,
0.575037484420216));
#37001=CARTESIAN_POINT('Ctrl Pts',(1.08246744900953E-15,-1.01946584908478,
0.567519513872719));
#37002=CARTESIAN_POINT('Ctrl Pts',(5.90599146279996E-16,-1.04866583648026,
0.526336362811751));
#37003=CARTESIAN_POINT('Ctrl Pts',(1.80552960326234E-15,-1.0752125083205,
0.483441946932646));
#37004=CARTESIAN_POINT('Ctrl Pts',(1.23859256184744E-15,-1.09893418145565,
0.439114326182033));
#37005=CARTESIAN_POINT('Ctrl Pts',(6.75767736099756E-16,-1.12248379203571,
0.395108230968164));
#37006=CARTESIAN_POINT('Ctrl Pts',(-8.48028993383386E-16,-1.14325009528961,
0.349688793728424));
#37007=CARTESIAN_POINT('Ctrl Pts',(-8.70831184940357E-16,-1.16103400319525,
0.303088562628634));
#37008=CARTESIAN_POINT('Ctrl Pts',(-8.92487487529703E-16,-1.17792420823819,
0.258830154268672));
#37009=CARTESIAN_POINT('Ctrl Pts',(-9.88970463367636E-16,-1.19212468288807,
0.21350576212291));
#37010=CARTESIAN_POINT('Ctrl Pts',(-9.29811783123569E-16,-1.20342780657952,
0.167291704370529));
#37011=CARTESIAN_POINT('Origin',(0.179677267864665,0.,0.));
#37012=CARTESIAN_POINT('',(-0.0506454642706703,0.,0.));
#37013=CARTESIAN_POINT('',(0.4,-0.733718498103797,8.98546010178019E-17));
#37014=CARTESIAN_POINT('',(0.179677267864665,-0.375,-4.59242549680257E-17));
#37015=CARTESIAN_POINT('Origin',(0.4,0.,0.));
#37016=CARTESIAN_POINT('Origin',(1.4,-1.38777878078145E-16,-0.866025403784439));
#37017=CARTESIAN_POINT('',(1.26393192622467,-1.59086285808736E-16,-0.866025403784439));
#37018=CARTESIAN_POINT('',(1.26393192622467,-0.75,-0.433012701892219));
#37019=CARTESIAN_POINT('Ctrl Pts',(1.26393192622467,-4.16333634234434E-16,
-0.866025403784438));
#37020=CARTESIAN_POINT('Ctrl Pts',(1.28128077719016,-0.128085793099759,
-0.792075036658926));
#37021=CARTESIAN_POINT('Ctrl Pts',(1.28802832775523,-0.255151508715124,
-0.718713611543623));
#37022=CARTESIAN_POINT('Ctrl Pts',(1.28802832775523,-0.494848491284876,
-0.580324494133036));
#37023=CARTESIAN_POINT('Ctrl Pts',(1.28128077719016,-0.621914206900241,
-0.506963069017732));
#37024=CARTESIAN_POINT('Ctrl Pts',(1.26393192622467,-0.75,-0.43301270189222));
#37025=CARTESIAN_POINT('',(0.4,-1.38777878078145E-16,-0.866025403784439));
#37026=CARTESIAN_POINT('',(1.4,-1.59086285808736E-16,-0.866025403784439));
#37027=CARTESIAN_POINT('',(0.4,-0.75,-0.433012701892219));
#37028=CARTESIAN_POINT('',(0.4,-0.75,-0.433012701892219));
#37029=CARTESIAN_POINT('',(1.4,-0.75,-0.433012701892219));
#37030=CARTESIAN_POINT('Origin',(1.4,-0.75,-0.433012701892219));
#37031=CARTESIAN_POINT('',(1.26393192622467,-0.75,0.433012701892219));
#37032=CARTESIAN_POINT('Ctrl Pts',(1.26393192622467,-0.75,-0.433012701892219));
#37033=CARTESIAN_POINT('Ctrl Pts',(1.28128077719016,-0.75,-0.285111967641195));
#37034=CARTESIAN_POINT('Ctrl Pts',(1.28802832775523,-0.75,-0.138389117410587));
#37035=CARTESIAN_POINT('Ctrl Pts',(1.28802832775523,-0.75,0.138389117410587));
#37036=CARTESIAN_POINT('Ctrl Pts',(1.28128077719016,-0.75,0.285111967641195));
#37037=CARTESIAN_POINT('Ctrl Pts',(1.26393192622467,-0.75,0.433012701892219));
#37038=CARTESIAN_POINT('',(0.4,-0.75,0.433012701892219));
#37039=CARTESIAN_POINT('',(0.4,-0.75,0.433012701892219));
#37040=CARTESIAN_POINT('',(1.4,-0.75,0.433012701892219));
#37041=CARTESIAN_POINT('Origin',(1.4,-0.75,0.433012701892219));
#37042=CARTESIAN_POINT('',(1.26393192622467,5.30287619362453E-17,0.866025403784439));
#37043=CARTESIAN_POINT('Ctrl Pts',(1.26393192622467,-0.75,0.433012701892219));
#37044=CARTESIAN_POINT('Ctrl Pts',(1.28128077719016,-0.621914206900242,
0.506963069017732));
#37045=CARTESIAN_POINT('Ctrl Pts',(1.28802832775523,-0.494848491284876,
0.580324494133036));
#37046=CARTESIAN_POINT('Ctrl Pts',(1.28802832775523,-0.255151508715124,
0.718713611543623));
#37047=CARTESIAN_POINT('Ctrl Pts',(1.28128077719016,-0.128085793099759,
0.792075036658926));
#37048=CARTESIAN_POINT('Ctrl Pts',(1.26393192622467,-2.42861286636753E-16,
0.866025403784438));
#37049=CARTESIAN_POINT('',(0.4,0.,0.866025403784439));
#37050=CARTESIAN_POINT('',(0.4,5.30287619362453E-17,0.866025403784439));
#37051=CARTESIAN_POINT('',(1.4,5.30287619362453E-17,0.866025403784439));
#37052=CARTESIAN_POINT('Origin',(1.4,0.,0.866025403784439));
#37053=CARTESIAN_POINT('',(1.26393192622467,0.75,0.433012701892219));
#37054=CARTESIAN_POINT('Ctrl Pts',(1.26393192622467,2.94902990916057E-16,
0.866025403784438));
#37055=CARTESIAN_POINT('Ctrl Pts',(1.28128077719016,0.128085793099758,0.792075036658926));
#37056=CARTESIAN_POINT('Ctrl Pts',(1.28802832775523,0.255151508715124,0.718713611543623));
#37057=CARTESIAN_POINT('Ctrl Pts',(1.28802832775523,0.494848491284876,0.580324494133036));
#37058=CARTESIAN_POINT('Ctrl Pts',(1.28128077719016,0.621914206900242,0.506963069017732));
#37059=CARTESIAN_POINT('Ctrl Pts',(1.26393192622467,0.75,0.433012701892219));
#37060=CARTESIAN_POINT('',(0.4,0.75,0.433012701892219));
#37061=CARTESIAN_POINT('',(0.4,0.75,0.433012701892219));
#37062=CARTESIAN_POINT('',(1.4,0.75,0.433012701892219));
#37063=CARTESIAN_POINT('Origin',(1.4,0.75,-0.43301270189222));
#37064=CARTESIAN_POINT('',(1.26393192622467,0.75,-0.43301270189222));
#37065=CARTESIAN_POINT('Ctrl Pts',(1.26393192622467,0.749999999999999,-0.43301270189222));
#37066=CARTESIAN_POINT('Ctrl Pts',(1.28128077719016,0.621914206900241,-0.506963069017732));
#37067=CARTESIAN_POINT('Ctrl Pts',(1.28802832775523,0.494848491284876,-0.580324494133036));
#37068=CARTESIAN_POINT('Ctrl Pts',(1.28802832775523,0.255151508715124,-0.718713611543623));
#37069=CARTESIAN_POINT('Ctrl Pts',(1.28128077719016,0.128085793099758,-0.792075036658926));
#37070=CARTESIAN_POINT('Ctrl Pts',(1.26393192622467,1.38777878078145E-16,
-0.866025403784438));
#37071=CARTESIAN_POINT('',(0.4,0.75,-0.43301270189222));
#37072=CARTESIAN_POINT('',(1.4,0.75,-0.43301270189222));
#37073=CARTESIAN_POINT('',(0.4,-1.59086285808736E-16,-0.866025403784439));
#37074=CARTESIAN_POINT('Origin',(1.4,0.75,0.433012701892219));
#37075=CARTESIAN_POINT('Ctrl Pts',(1.26393192622467,0.75,0.433012701892219));
#37076=CARTESIAN_POINT('Ctrl Pts',(1.28128077719016,0.75,0.285111967641195));
#37077=CARTESIAN_POINT('Ctrl Pts',(1.28802832775523,0.75,0.138389117410587));
#37078=CARTESIAN_POINT('Ctrl Pts',(1.28802832775523,0.75,-0.138389117410587));
#37079=CARTESIAN_POINT('Ctrl Pts',(1.28128077719016,0.75,-0.285111967641195));
#37080=CARTESIAN_POINT('Ctrl Pts',(1.26393192622467,0.75,-0.433012701892219));
#37081=CARTESIAN_POINT('',(0.4,0.75,-0.43301270189222));
#37082=CARTESIAN_POINT('Origin',(0.4,0.,0.));
#37083=CARTESIAN_POINT('Origin',(-8.,1.,0.));
#37084=CARTESIAN_POINT('',(-8.,-1.,-1.22464679914735E-16));
#37085=CARTESIAN_POINT('Origin',(-8.,0.,0.));
#37086=CARTESIAN_POINT('Origin',(-7.875,0.,0.));
#37087=CARTESIAN_POINT('',(-7.875,-1.125,-1.37772764904077E-16));
#37088=CARTESIAN_POINT('Origin',(-3.875,0.,0.));
#37089=CARTESIAN_POINT('Origin',(0.,0.,0.));
#37090=CARTESIAN_POINT('Origin',(0.,2.35,0.));
#37091=CARTESIAN_POINT('',(-8.67361737988404E-18,-2.35,-2.87791997799628E-16));
#37092=CARTESIAN_POINT('Origin',(0.,0.,0.));
#37093=CARTESIAN_POINT('Origin',(0.0749999999999999,0.,0.));
#37094=CARTESIAN_POINT('',(0.15,-2.35,-2.87791997799628E-16));
#37095=CARTESIAN_POINT('',(0.15,-2.87791997799628E-16,2.35));
#37096=CARTESIAN_POINT('Origin',(0.15,0.,0.));
#37097=CARTESIAN_POINT('',(0.0749999999999999,-2.35,-2.87791997799628E-16));
#37098=CARTESIAN_POINT('Origin',(0.15,0.,0.));
#37099=CARTESIAN_POINT('Ctrl Pts',(0.15,0.,2.35));
#37100=CARTESIAN_POINT('Ctrl Pts',(0.15,-2.35,2.35));
#37101=CARTESIAN_POINT('Ctrl Pts',(0.15,-2.35,0.));
#37102=CARTESIAN_POINT('Ctrl Pts',(0.15,-2.35,-2.35));
#37103=CARTESIAN_POINT('Ctrl Pts',(0.15,0.,-2.35));
#37104=CARTESIAN_POINT('Ctrl Pts',(0.15,2.35,-2.35));
#37105=CARTESIAN_POINT('Ctrl Pts',(0.15,2.35,0.));
#37106=CARTESIAN_POINT('Ctrl Pts',(0.15,2.35,2.35));
#37107=CARTESIAN_POINT('Ctrl Pts',(0.15,0.,2.35));
#37108=CARTESIAN_POINT('Ctrl Pts',(1.09479837717015,0.,1.81728317490632));
#37109=CARTESIAN_POINT('Ctrl Pts',(1.09479837717015,-1.81728317490632,1.81728317490632));
#37110=CARTESIAN_POINT('Ctrl Pts',(1.09479837717015,-1.81728317490632,0.));
#37111=CARTESIAN_POINT('Ctrl Pts',(1.09479837717015,-1.81728317490632,-1.81728317490632));
#37112=CARTESIAN_POINT('Ctrl Pts',(1.09479837717015,0.,-1.81728317490632));
#37113=CARTESIAN_POINT('Ctrl Pts',(1.09479837717015,1.81728317490632,-1.81728317490632));
#37114=CARTESIAN_POINT('Ctrl Pts',(1.09479837717015,1.81728317490632,0.));
#37115=CARTESIAN_POINT('Ctrl Pts',(1.09479837717015,1.81728317490632,1.81728317490632));
#37116=CARTESIAN_POINT('Ctrl Pts',(1.09479837717015,0.,1.81728317490632));
#37117=CARTESIAN_POINT('Ctrl Pts',(1.28802832775523,0.,0.75));
#37118=CARTESIAN_POINT('Ctrl Pts',(1.28802832775523,-0.75,0.75));
#37119=CARTESIAN_POINT('Ctrl Pts',(1.28802832775523,-0.75,0.));
#37120=CARTESIAN_POINT('Ctrl Pts',(1.28802832775523,-0.75,-0.75));
#37121=CARTESIAN_POINT('Ctrl Pts',(1.28802832775523,0.,-0.75));
#37122=CARTESIAN_POINT('Ctrl Pts',(1.28802832775523,0.75,-0.75));
#37123=CARTESIAN_POINT('Ctrl Pts',(1.28802832775523,0.75,0.));
#37124=CARTESIAN_POINT('Ctrl Pts',(1.28802832775523,0.75,0.75));
#37125=CARTESIAN_POINT('Ctrl Pts',(1.28802832775523,0.,0.75));
#37126=CARTESIAN_POINT('Ctrl Pts',(1.26393192622467,0.,0.86602540378444));
#37127=CARTESIAN_POINT('Ctrl Pts',(1.03252872779688,0.,1.85239340658685));
#37128=CARTESIAN_POINT('Ctrl Pts',(0.15,0.,2.35));
#37129=CARTESIAN_POINT('',(0.,0.,0.));
#37130=CARTESIAN_POINT('',(0.,0.,0.));
#37131=CARTESIAN_POINT('',(0.,0.,0.));
#37132=CARTESIAN_POINT('',(0.,0.,0.));
#37133=CARTESIAN_POINT('',(0.,0.,0.));
#37134=CARTESIAN_POINT('',(0.,0.,0.));
#37135=CARTESIAN_POINT('',(24.,-7.88860905221012E-30,-47.5));
#37136=CARTESIAN_POINT('',(34.4,0.,-33.));
#37137=CARTESIAN_POINT('',(34.4,0.,-33.));
#37138=CARTESIAN_POINT('',(25.2,1.33226762955019E-14,-33.));
#37139=CARTESIAN_POINT('',(39.5,0.,6.));
#37140=CARTESIAN_POINT('',(39.5,0.,6.8));
#37141=CARTESIAN_POINT('',(39.5,0.,-6.));
#37142=CARTESIAN_POINT('',(39.5,0.,-6.8));
#37143=CARTESIAN_POINT('',(-34.4,0.,-33.));
#37144=CARTESIAN_POINT('',(-34.4,0.,-33.));
#37145=CARTESIAN_POINT('',(-25.2,1.33226762955019E-14,-33.));
#37146=CARTESIAN_POINT('',(-39.5,0.,6.));
#37147=CARTESIAN_POINT('',(-39.5,0.,6.8));
#37148=CARTESIAN_POINT('',(-39.5,0.,-6.));
#37149=CARTESIAN_POINT('',(-39.5,0.,-6.8));
#37150=CARTESIAN_POINT('',(-34.25,11.,-47.5));
#37151=CARTESIAN_POINT('',(42.25,11.,-47.5));
#37152=UNCERTAINTY_MEASURE_WITH_UNIT(LENGTH_MEASURE(0.01),#37182,
'DISTANCE_ACCURACY_VALUE',
'Maximum model space distance between geometric entities at asserted c
onnectivities');
#37153=UNCERTAINTY_MEASURE_WITH_UNIT(LENGTH_MEASURE(0.01),#37182,
'DISTANCE_ACCURACY_VALUE',
'Maximum model space distance between geometric entities at asserted c
onnectivities');
#37154=UNCERTAINTY_MEASURE_WITH_UNIT(LENGTH_MEASURE(0.01),#37182,
'DISTANCE_ACCURACY_VALUE',
'Maximum model space distance between geometric entities at asserted c
onnectivities');
#37155=UNCERTAINTY_MEASURE_WITH_UNIT(LENGTH_MEASURE(0.01),#37182,
'DISTANCE_ACCURACY_VALUE',
'Maximum model space distance between geometric entities at asserted c
onnectivities');
#37156=UNCERTAINTY_MEASURE_WITH_UNIT(LENGTH_MEASURE(0.01),#37182,
'DISTANCE_ACCURACY_VALUE',
'Maximum model space distance between geometric entities at asserted c
onnectivities');
#37157=UNCERTAINTY_MEASURE_WITH_UNIT(LENGTH_MEASURE(0.01),#37182,
'DISTANCE_ACCURACY_VALUE',
'Maximum model space distance between geometric entities at asserted c
onnectivities');
#37158=UNCERTAINTY_MEASURE_WITH_UNIT(LENGTH_MEASURE(0.01),#37182,
'DISTANCE_ACCURACY_VALUE',
'Maximum model space distance between geometric entities at asserted c
onnectivities');
#37159=UNCERTAINTY_MEASURE_WITH_UNIT(LENGTH_MEASURE(0.01),#37182,
'DISTANCE_ACCURACY_VALUE',
'Maximum model space distance between geometric entities at asserted c
onnectivities');
#37160=UNCERTAINTY_MEASURE_WITH_UNIT(LENGTH_MEASURE(0.01),#37182,
'DISTANCE_ACCURACY_VALUE',
'Maximum model space distance between geometric entities at asserted c
onnectivities');
#37161=UNCERTAINTY_MEASURE_WITH_UNIT(LENGTH_MEASURE(0.01),#37182,
'DISTANCE_ACCURACY_VALUE',
'Maximum model space distance between geometric entities at asserted c
onnectivities');
#37162=UNCERTAINTY_MEASURE_WITH_UNIT(LENGTH_MEASURE(0.01),#37182,
'DISTANCE_ACCURACY_VALUE',
'Maximum model space distance between geometric entities at asserted c
onnectivities');
#37163=UNCERTAINTY_MEASURE_WITH_UNIT(LENGTH_MEASURE(0.01),#37182,
'DISTANCE_ACCURACY_VALUE',
'Maximum model space distance between geometric entities at asserted c
onnectivities');
#37164=UNCERTAINTY_MEASURE_WITH_UNIT(LENGTH_MEASURE(0.01),#37182,
'DISTANCE_ACCURACY_VALUE',
'Maximum model space distance between geometric entities at asserted c
onnectivities');
#37165=UNCERTAINTY_MEASURE_WITH_UNIT(LENGTH_MEASURE(0.01),#37182,
'DISTANCE_ACCURACY_VALUE',
'Maximum model space distance between geometric entities at asserted c
onnectivities');
#37166=UNCERTAINTY_MEASURE_WITH_UNIT(LENGTH_MEASURE(0.01),#37182,
'DISTANCE_ACCURACY_VALUE',
'Maximum model space distance between geometric entities at asserted c
onnectivities');
#37167=(
GEOMETRIC_REPRESENTATION_CONTEXT(3)
GLOBAL_UNCERTAINTY_ASSIGNED_CONTEXT((#37152))
GLOBAL_UNIT_ASSIGNED_CONTEXT((#37182,#37184,#37185))
REPRESENTATION_CONTEXT('','3D')
);
#37168=(
GEOMETRIC_REPRESENTATION_CONTEXT(3)
GLOBAL_UNCERTAINTY_ASSIGNED_CONTEXT((#37153))
GLOBAL_UNIT_ASSIGNED_CONTEXT((#37182,#37184,#37185))
REPRESENTATION_CONTEXT('','3D')
);
#37169=(
GEOMETRIC_REPRESENTATION_CONTEXT(3)
GLOBAL_UNCERTAINTY_ASSIGNED_CONTEXT((#37154))
GLOBAL_UNIT_ASSIGNED_CONTEXT((#37182,#37184,#37185))
REPRESENTATION_CONTEXT('','3D')
);
#37170=(
GEOMETRIC_REPRESENTATION_CONTEXT(3)
GLOBAL_UNCERTAINTY_ASSIGNED_CONTEXT((#37155))
GLOBAL_UNIT_ASSIGNED_CONTEXT((#37182,#37184,#37185))
REPRESENTATION_CONTEXT('','3D')
);
#37171=(
GEOMETRIC_REPRESENTATION_CONTEXT(3)
GLOBAL_UNCERTAINTY_ASSIGNED_CONTEXT((#37156))
GLOBAL_UNIT_ASSIGNED_CONTEXT((#37182,#37184,#37185))
REPRESENTATION_CONTEXT('','3D')
);
#37172=(
GEOMETRIC_REPRESENTATION_CONTEXT(3)
GLOBAL_UNCERTAINTY_ASSIGNED_CONTEXT((#37157))
GLOBAL_UNIT_ASSIGNED_CONTEXT((#37182,#37184,#37185))
REPRESENTATION_CONTEXT('','3D')
);
#37173=(
GEOMETRIC_REPRESENTATION_CONTEXT(3)
GLOBAL_UNCERTAINTY_ASSIGNED_CONTEXT((#37158))
GLOBAL_UNIT_ASSIGNED_CONTEXT((#37182,#37184,#37185))
REPRESENTATION_CONTEXT('','3D')
);
#37174=(
GEOMETRIC_REPRESENTATION_CONTEXT(3)
GLOBAL_UNCERTAINTY_ASSIGNED_CONTEXT((#37159))
GLOBAL_UNIT_ASSIGNED_CONTEXT((#37182,#37184,#37185))
REPRESENTATION_CONTEXT('','3D')
);
#37175=(
GEOMETRIC_REPRESENTATION_CONTEXT(3)
GLOBAL_UNCERTAINTY_ASSIGNED_CONTEXT((#37160))
GLOBAL_UNIT_ASSIGNED_CONTEXT((#37182,#37184,#37185))
REPRESENTATION_CONTEXT('','3D')
);
#37176=(
GEOMETRIC_REPRESENTATION_CONTEXT(3)
GLOBAL_UNCERTAINTY_ASSIGNED_CONTEXT((#37161))
GLOBAL_UNIT_ASSIGNED_CONTEXT((#37182,#37184,#37185))
REPRESENTATION_CONTEXT('','3D')
);
#37177=(
GEOMETRIC_REPRESENTATION_CONTEXT(3)
GLOBAL_UNCERTAINTY_ASSIGNED_CONTEXT((#37162))
GLOBAL_UNIT_ASSIGNED_CONTEXT((#37182,#37184,#37185))
REPRESENTATION_CONTEXT('','3D')
);
#37178=(
GEOMETRIC_REPRESENTATION_CONTEXT(3)
GLOBAL_UNCERTAINTY_ASSIGNED_CONTEXT((#37163))
GLOBAL_UNIT_ASSIGNED_CONTEXT((#37182,#37184,#37185))
REPRESENTATION_CONTEXT('','3D')
);
#37179=(
GEOMETRIC_REPRESENTATION_CONTEXT(3)
GLOBAL_UNCERTAINTY_ASSIGNED_CONTEXT((#37164))
GLOBAL_UNIT_ASSIGNED_CONTEXT((#37182,#37184,#37185))
REPRESENTATION_CONTEXT('','3D')
);
#37180=(
GEOMETRIC_REPRESENTATION_CONTEXT(3)
GLOBAL_UNCERTAINTY_ASSIGNED_CONTEXT((#37165))
GLOBAL_UNIT_ASSIGNED_CONTEXT((#37182,#37184,#37185))
REPRESENTATION_CONTEXT('','3D')
);
#37181=(
GEOMETRIC_REPRESENTATION_CONTEXT(3)
GLOBAL_UNCERTAINTY_ASSIGNED_CONTEXT((#37166))
GLOBAL_UNIT_ASSIGNED_CONTEXT((#37182,#37184,#37185))
REPRESENTATION_CONTEXT('','3D')
);
#37182=(
LENGTH_UNIT()
NAMED_UNIT(*)
SI_UNIT(.MILLI.,.METRE.)
);
#37183=(
LENGTH_UNIT()
NAMED_UNIT(*)
SI_UNIT($,.METRE.)
);
#37184=(
NAMED_UNIT(*)
PLANE_ANGLE_UNIT()
SI_UNIT($,.RADIAN.)
);
#37185=(
NAMED_UNIT(*)
SI_UNIT($,.STERADIAN.)
SOLID_ANGLE_UNIT()
);
#37186=SHAPE_DEFINITION_REPRESENTATION(#37200,#37237);
#37187=SHAPE_DEFINITION_REPRESENTATION(#37201,#37238);
#37188=SHAPE_DEFINITION_REPRESENTATION(#37202,#37239);
#37189=SHAPE_DEFINITION_REPRESENTATION(#37203,#37240);
#37190=SHAPE_DEFINITION_REPRESENTATION(#37204,#37241);
#37191=SHAPE_DEFINITION_REPRESENTATION(#37205,#37242);
#37192=SHAPE_DEFINITION_REPRESENTATION(#37206,#37243);
#37193=SHAPE_DEFINITION_REPRESENTATION(#37207,#37244);
#37194=SHAPE_DEFINITION_REPRESENTATION(#37208,#37245);
#37195=SHAPE_DEFINITION_REPRESENTATION(#37209,#37246);
#37196=SHAPE_DEFINITION_REPRESENTATION(#37210,#37247);
#37197=SHAPE_DEFINITION_REPRESENTATION(#37211,#37248);
#37198=SHAPE_DEFINITION_REPRESENTATION(#37212,#37249);
#37199=SHAPE_DEFINITION_REPRESENTATION(#37213,#37250);
#37200=PRODUCT_DEFINITION_SHAPE('',$,#37252);
#37201=PRODUCT_DEFINITION_SHAPE('',$,#37253);
#37202=PRODUCT_DEFINITION_SHAPE('',$,#37254);
#37203=PRODUCT_DEFINITION_SHAPE('',$,#37255);
#37204=PRODUCT_DEFINITION_SHAPE('',$,#37256);
#37205=PRODUCT_DEFINITION_SHAPE('',$,#37257);
#37206=PRODUCT_DEFINITION_SHAPE('',$,#37258);
#37207=PRODUCT_DEFINITION_SHAPE('',$,#37259);
#37208=PRODUCT_DEFINITION_SHAPE('',$,#37260);
#37209=PRODUCT_DEFINITION_SHAPE('',$,#37261);
#37210=PRODUCT_DEFINITION_SHAPE('',$,#37262);
#37211=PRODUCT_DEFINITION_SHAPE('',$,#37263);
#37212=PRODUCT_DEFINITION_SHAPE('',$,#37264);
#37213=PRODUCT_DEFINITION_SHAPE('',$,#37265);
#37214=PRODUCT_DEFINITION_SHAPE($,$,#80);
#37215=PRODUCT_DEFINITION_SHAPE($,$,#81);
#37216=PRODUCT_DEFINITION_SHAPE($,$,#82);
#37217=PRODUCT_DEFINITION_SHAPE($,$,#83);
#37218=PRODUCT_DEFINITION_SHAPE($,$,#84);
#37219=PRODUCT_DEFINITION_SHAPE($,$,#85);
#37220=PRODUCT_DEFINITION_SHAPE($,$,#86);
#37221=PRODUCT_DEFINITION_SHAPE($,$,#87);
#37222=PRODUCT_DEFINITION_SHAPE($,$,#88);
#37223=PRODUCT_DEFINITION_SHAPE($,$,#89);
#37224=PRODUCT_DEFINITION_SHAPE($,$,#90);
#37225=PRODUCT_DEFINITION_SHAPE($,$,#91);
#37226=PRODUCT_DEFINITION_SHAPE($,$,#92);
#37227=PRODUCT_DEFINITION_SHAPE($,$,#93);
#37228=PRODUCT_DEFINITION_SHAPE($,$,#94);
#37229=PRODUCT_DEFINITION_SHAPE($,$,#95);
#37230=PRODUCT_DEFINITION_SHAPE($,$,#96);
#37231=PRODUCT_DEFINITION_SHAPE($,$,#97);
#37232=PRODUCT_DEFINITION_SHAPE($,$,#98);
#37233=PRODUCT_DEFINITION_SHAPE($,$,#99);
#37234=PRODUCT_DEFINITION_SHAPE($,$,#100);
#37235=PRODUCT_DEFINITION_SHAPE($,$,#101);
#37236=PRODUCT_DEFINITION_SHAPE($,$,#102);
#37237=SHAPE_REPRESENTATION('',(#14933,#16102,#16103,#16104,#16105,#16106,
#16107,#16108,#16109,#16110,#16111,#16112,#16113,#16114,#16115,#16116,#16117,
#16118,#16119,#16120,#16121,#16122,#16123,#16124),#37167);
#37238=SHAPE_REPRESENTATION('',(#14934),#37168);
#37239=SHAPE_REPRESENTATION('',(#14997),#37169);
#37240=SHAPE_REPRESENTATION('',(#15137),#37170);
#37241=SHAPE_REPRESENTATION('',(#15323),#37171);
#37242=SHAPE_REPRESENTATION('',(#15403),#37172);
#37243=SHAPE_REPRESENTATION('',(#15425),#37173);
#37244=SHAPE_REPRESENTATION('',(#15455),#37174);
#37245=SHAPE_REPRESENTATION('',(#15705),#37175);
#37246=SHAPE_REPRESENTATION('',(#15848),#37176);
#37247=SHAPE_REPRESENTATION('',(#15916),#37177);
#37248=SHAPE_REPRESENTATION('',(#15999),#37178);
#37249=SHAPE_REPRESENTATION('',(#16013),#37179);
#37250=SHAPE_REPRESENTATION('',(#16039),#37180);
#37251=PRODUCT_DEFINITION_CONTEXT('part definition',#37295,'design');
#37252=PRODUCT_DEFINITION('2026-10-20-13-23-46-240','MAS-287',#37266,#37251);
#37253=PRODUCT_DEFINITION('2026-10-20-13-23-47-382',
'01_Clamp_Upper_Half_PLA',#37267,#37251);
#37254=PRODUCT_DEFINITION('2026-10-20-13-23-47-919',
'02_Clamp_Lower_Half_with_Legs_PLA',#37268,#37251);
#37255=PRODUCT_DEFINITION('2026-10-20-13-23-49-638',
'03_Camera_Housing_Body_PLA',#37269,#37251);
#37256=PRODUCT_DEFINITION('2026-10-20-13-23-53-005',
'04_Camera_Housing_Front_Cover_PLA',#37270,#37251);
#37257=PRODUCT_DEFINITION('2026-10-20-13-23-54-211','05_USB_Camera_PCB',
#37271,#37251);
#37258=PRODUCT_DEFINITION('2026-10-20-13-23-55-996','06_M8_Lens_Holder',
#37272,#37251);
#37259=PRODUCT_DEFINITION('2026-10-20-13-23-56-870','07_M8_Camera_Lens',
#37273,#37251);
#37260=PRODUCT_DEFINITION('2026-10-20-13-23-58-415',
'08_Knurled_Thumb_Knob_PLA',#37274,#37251);
#37261=PRODUCT_DEFINITION('2026-10-20-13-23-59-935','09_ISO_4017_M4x16',
#37275,#37251);
#37262=PRODUCT_DEFINITION('2026-10-20-13-24-03-042','11_ISO_7380_M4x20',
#37276,#37251);
#37263=PRODUCT_DEFINITION('2026-10-20-13-24-04-900',
'12_ISO_7089_Washer_M4',#37277,#37251);
#37264=PRODUCT_DEFINITION('2026-10-20-13-24-01-496',
'10_ISO_4032_Nut_M4',#37278,#37251);
#37265=PRODUCT_DEFINITION('2026-10-20-13-24-05-459',
'13_ISO_7380_M2.5x8',#37279,#37251);
#37266=PRODUCT_DEFINITION_FORMATION('',$,#37297);
#37267=PRODUCT_DEFINITION_FORMATION('',$,#37298);
#37268=PRODUCT_DEFINITION_FORMATION('',$,#37299);
#37269=PRODUCT_DEFINITION_FORMATION('',$,#37300);
#37270=PRODUCT_DEFINITION_FORMATION('',$,#37301);
#37271=PRODUCT_DEFINITION_FORMATION('',$,#37302);
#37272=PRODUCT_DEFINITION_FORMATION('',$,#37303);
#37273=PRODUCT_DEFINITION_FORMATION('',$,#37304);
#37274=PRODUCT_DEFINITION_FORMATION('',$,#37305);
#37275=PRODUCT_DEFINITION_FORMATION('',$,#37306);
#37276=PRODUCT_DEFINITION_FORMATION('',$,#37307);
#37277=PRODUCT_DEFINITION_FORMATION('',$,#37308);
#37278=PRODUCT_DEFINITION_FORMATION('',$,#37309);
#37279=PRODUCT_DEFINITION_FORMATION('',$,#37310);
#37280=PRODUCT_RELATED_PRODUCT_CATEGORY('MAS-287','MAS-287',(#37297));
#37281=PRODUCT_RELATED_PRODUCT_CATEGORY('01_Clamp_Upper_Half_PLA',
'01_Clamp_Upper_Half_PLA',(#37298));
#37282=PRODUCT_RELATED_PRODUCT_CATEGORY(
'02_Clamp_Lower_Half_with_Legs_PLA','02_Clamp_Lower_Half_with_Legs_PLA',
(#37299));
#37283=PRODUCT_RELATED_PRODUCT_CATEGORY('03_Camera_Housing_Body_PLA',
'03_Camera_Housing_Body_PLA',(#37300));
#37284=PRODUCT_RELATED_PRODUCT_CATEGORY(
'04_Camera_Housing_Front_Cover_PLA','04_Camera_Housing_Front_Cover_PLA',
(#37301));
#37285=PRODUCT_RELATED_PRODUCT_CATEGORY('05_USB_Camera_PCB',
'05_USB_Camera_PCB',(#37302));
#37286=PRODUCT_RELATED_PRODUCT_CATEGORY('06_M8_Lens_Holder',
'06_M8_Lens_Holder',(#37303));
#37287=PRODUCT_RELATED_PRODUCT_CATEGORY('07_M8_Camera_Lens',
'07_M8_Camera_Lens',(#37304));
#37288=PRODUCT_RELATED_PRODUCT_CATEGORY('08_Knurled_Thumb_Knob_PLA',
'08_Knurled_Thumb_Knob_PLA',(#37305));
#37289=PRODUCT_RELATED_PRODUCT_CATEGORY('09_ISO_4017_M4x16',
'09_ISO_4017_M4x16',(#37306));
#37290=PRODUCT_RELATED_PRODUCT_CATEGORY('11_ISO_7380_M4x20',
'11_ISO_7380_M4x20',(#37307));
#37291=PRODUCT_RELATED_PRODUCT_CATEGORY('12_ISO_7089_Washer_M4',
'12_ISO_7089_Washer_M4',(#37308));
#37292=PRODUCT_RELATED_PRODUCT_CATEGORY('10_ISO_4032_Nut_M4',
'10_ISO_4032_Nut_M4',(#37309));
#37293=PRODUCT_RELATED_PRODUCT_CATEGORY('13_ISO_7380_M2.5x8',
'13_ISO_7380_M2.5x8',(#37310));
#37294=APPLICATION_PROTOCOL_DEFINITION('international standard',
'automotive_design',2009,#37295);
#37295=APPLICATION_CONTEXT(
'Core Data for Automotive Mechanical Design Process');
#37296=PRODUCT_CONTEXT('part definition',#37295,'mechanical');
#37297=PRODUCT('2026-10-20-13-23-46-240','MAS-287',$,(#37296));
#37298=PRODUCT('2026-10-20-13-23-47-382','01_Clamp_Upper_Half_PLA',$,(#37296));
#37299=PRODUCT('2026-10-20-13-23-47-919',
'02_Clamp_Lower_Half_with_Legs_PLA',$,(#37296));
#37300=PRODUCT('2026-10-20-13-23-49-638','03_Camera_Housing_Body_PLA',$,
(#37296));
#37301=PRODUCT('2026-10-20-13-23-53-005',
'04_Camera_Housing_Front_Cover_PLA',$,(#37296));
#37302=PRODUCT('2026-10-20-13-23-54-211','05_USB_Camera_PCB',$,(#37296));
#37303=PRODUCT('2026-10-20-13-23-55-996','06_M8_Lens_Holder',$,(#37296));
#37304=PRODUCT('2026-10-20-13-23-56-870','07_M8_Camera_Lens',$,(#37296));
#37305=PRODUCT('2026-10-20-13-23-58-415','08_Knurled_Thumb_Knob_PLA',$,
(#37296));
#37306=PRODUCT('2026-10-20-13-23-59-935','09_ISO_4017_M4x16',$,(#37296));
#37307=PRODUCT('2026-10-20-13-24-03-042','11_ISO_7380_M4x20',$,(#37296));
#37308=PRODUCT('2026-10-20-13-24-04-900','12_ISO_7089_Washer_M4',$,(#37296));
#37309=PRODUCT('2026-10-20-13-24-01-496','10_ISO_4032_Nut_M4',$,(#37296));
#37310=PRODUCT('2026-10-20-13-24-05-459','13_ISO_7380_M2.5x8',$,(#37296));
#37311=PRESENTATION_STYLE_ASSIGNMENT((#37316));
#37312=PRESENTATION_STYLE_ASSIGNMENT((#37317));
#37313=PRESENTATION_STYLE_ASSIGNMENT((#37318));
#37314=PRESENTATION_STYLE_ASSIGNMENT((#37319));
#37315=PRESENTATION_STYLE_ASSIGNMENT((#37320));
#37316=SURFACE_STYLE_USAGE(.BOTH.,#37321);
#37317=SURFACE_STYLE_USAGE(.BOTH.,#37322);
#37318=SURFACE_STYLE_USAGE(.BOTH.,#37323);
#37319=SURFACE_STYLE_USAGE(.BOTH.,#37324);
#37320=SURFACE_STYLE_USAGE(.BOTH.,#37325);
#37321=SURFACE_SIDE_STYLE('',(#37326));
#37322=SURFACE_SIDE_STYLE('',(#37327));
#37323=SURFACE_SIDE_STYLE('',(#37328));
#37324=SURFACE_SIDE_STYLE('',(#37329));
#37325=SURFACE_SIDE_STYLE('',(#37330));
#37326=SURFACE_STYLE_FILL_AREA(#37331);
#37327=SURFACE_STYLE_FILL_AREA(#37332);
#37328=SURFACE_STYLE_FILL_AREA(#37333);
#37329=SURFACE_STYLE_FILL_AREA(#37334);
#37330=SURFACE_STYLE_FILL_AREA(#37335);
#37331=FILL_AREA_STYLE('Steel - Satin',(#37336));
#37332=FILL_AREA_STYLE('MAS287_gun',(#37337));
#37333=FILL_AREA_STYLE('MAS287_ti',(#37338));
#37334=FILL_AREA_STYLE('MAS287_al',(#37339));
#37335=FILL_AREA_STYLE('MAS287_ss',(#37340));
#37336=FILL_AREA_STYLE_COLOUR('Steel - Satin',#37341);
#37337=FILL_AREA_STYLE_COLOUR('MAS287_gun',#37342);
#37338=FILL_AREA_STYLE_COLOUR('MAS287_ti',#37343);
#37339=FILL_AREA_STYLE_COLOUR('MAS287_al',#37344);
#37340=FILL_AREA_STYLE_COLOUR('MAS287_ss',#37345);
#37341=COLOUR_RGB('Steel - Satin',0.627450980392157,0.627450980392157,0.627450980392157);
#37342=COLOUR_RGB('MAS287_gun',0.313725490196078,0.337254901960784,0.364705882352941);
#37343=COLOUR_RGB('MAS287_ti',0.549019607843137,0.572549019607843,0.596078431372549);
#37344=COLOUR_RGB('MAS287_al',0.67843137254902,0.705882352941177,0.729411764705882);
#37345=COLOUR_RGB('MAS287_ss',0.83921568627451,0.850980392156863,0.862745098039216);
#37346=COLOUR_RGB('Dark Blue',0.08,0.2,0.34);
#37347=FILL_AREA_STYLE_COLOUR('',#37346);
#37348=FILL_AREA_STYLE('',(#37347));
#37349=SURFACE_STYLE_FILL_AREA(#37348);
#37350=SURFACE_SIDE_STYLE('',(#37349));
#37351=SURFACE_STYLE_USAGE(.BOTH.,#37350);
#37352=PRESENTATION_STYLE_ASSIGNMENT((#37351));
#37353=COLOUR_RGB('Light Blue',0.38,0.62,0.78);
#37354=FILL_AREA_STYLE_COLOUR('',#37353);
#37355=FILL_AREA_STYLE('',(#37354));
#37356=SURFACE_STYLE_FILL_AREA(#37355);
#37357=SURFACE_SIDE_STYLE('',(#37356));
#37358=SURFACE_STYLE_USAGE(.BOTH.,#37357);
#37359=PRESENTATION_STYLE_ASSIGNMENT((#37358));
#37360=COLOUR_RGB('Sky Blue',0.24,0.69,0.87);
#37361=FILL_AREA_STYLE_COLOUR('',#37360);
#37362=FILL_AREA_STYLE('',(#37361));
#37363=SURFACE_STYLE_FILL_AREA(#37362);
#37364=SURFACE_SIDE_STYLE('',(#37363));
#37365=SURFACE_STYLE_USAGE(.BOTH.,#37364);
#37366=PRESENTATION_STYLE_ASSIGNMENT((#37365));
#37367=COLOUR_RGB('Grey',0.48,0.52,0.57);
#37368=FILL_AREA_STYLE_COLOUR('',#37367);
#37369=FILL_AREA_STYLE('',(#37368));
#37370=SURFACE_STYLE_FILL_AREA(#37369);
#37371=SURFACE_SIDE_STYLE('',(#37370));
#37372=SURFACE_STYLE_USAGE(.BOTH.,#37371);
#37373=PRESENTATION_STYLE_ASSIGNMENT((#37372));
#37374=COLOUR_RGB('Black',0.12,0.14,0.17);
#37375=FILL_AREA_STYLE_COLOUR('',#37374);
#37376=FILL_AREA_STYLE('',(#37375));
#37377=SURFACE_STYLE_FILL_AREA(#37376);
#37378=SURFACE_SIDE_STYLE('',(#37377));
#37379=SURFACE_STYLE_USAGE(.BOTH.,#37378);
#37380=PRESENTATION_STYLE_ASSIGNMENT((#37379));
#37381=COLOUR_RGB('Off White',0.89,0.88,0.83);
#37382=FILL_AREA_STYLE_COLOUR('',#37381);
#37383=FILL_AREA_STYLE('',(#37382));
#37384=SURFACE_STYLE_FILL_AREA(#37383);
#37385=SURFACE_SIDE_STYLE('',(#37384));
#37386=SURFACE_STYLE_USAGE(.BOTH.,#37385);
#37387=PRESENTATION_STYLE_ASSIGNMENT((#37386));
ENDSEC;
END-ISO-10303-21;
